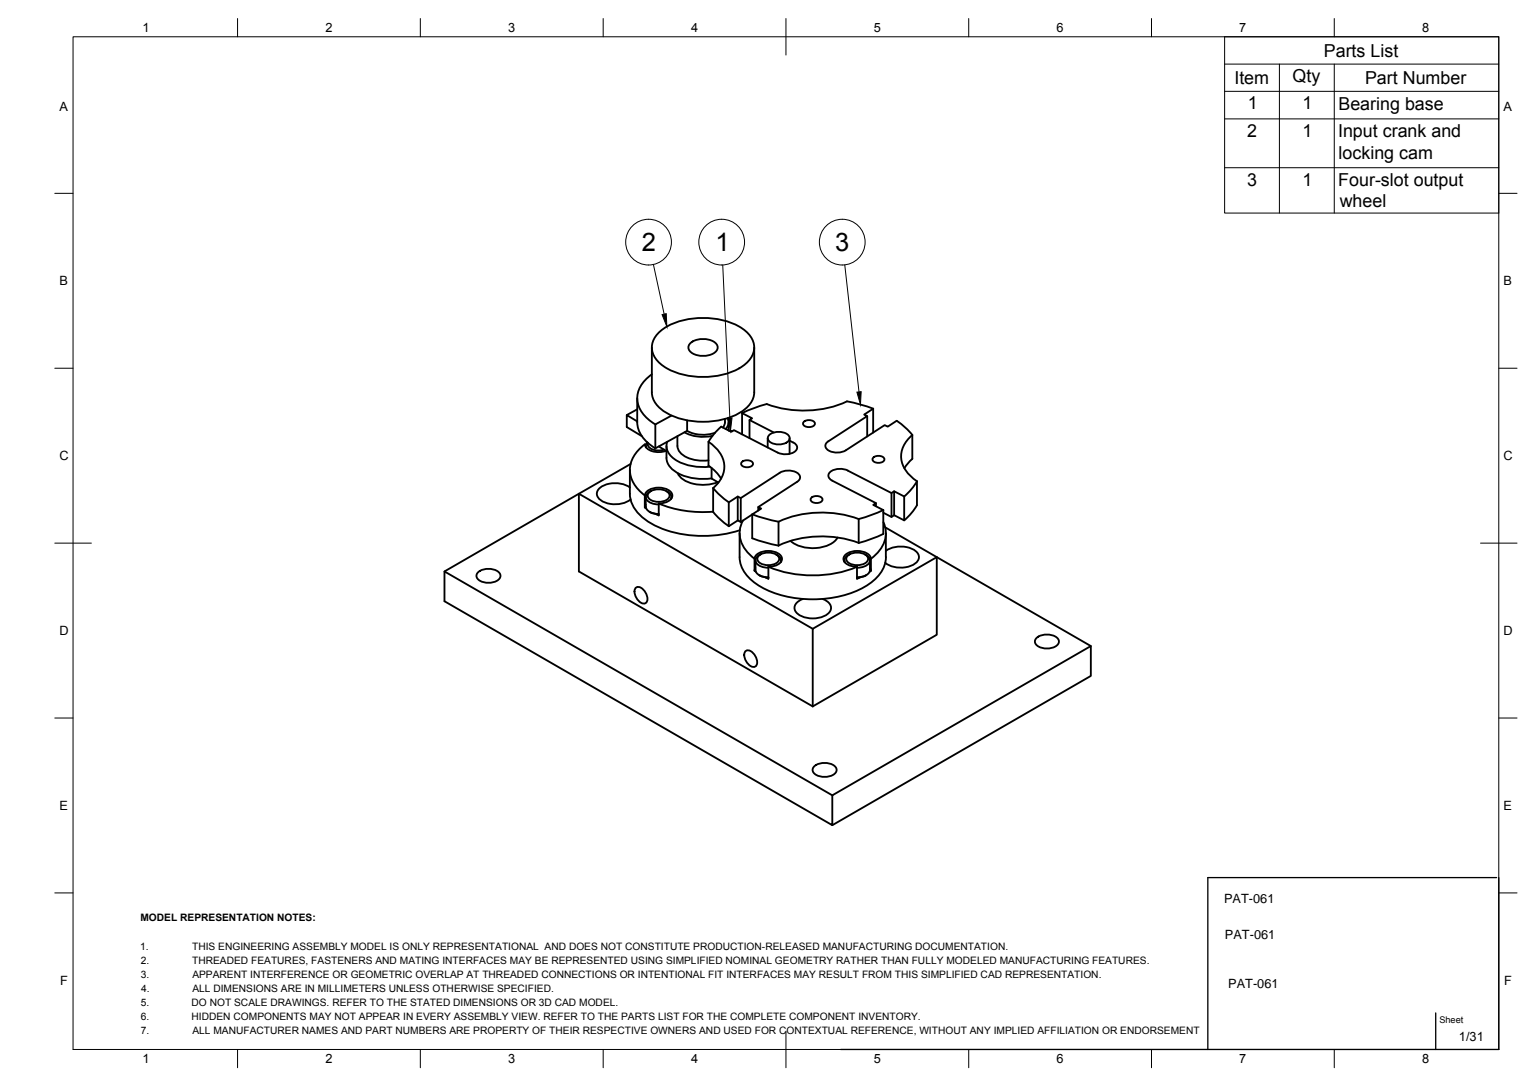
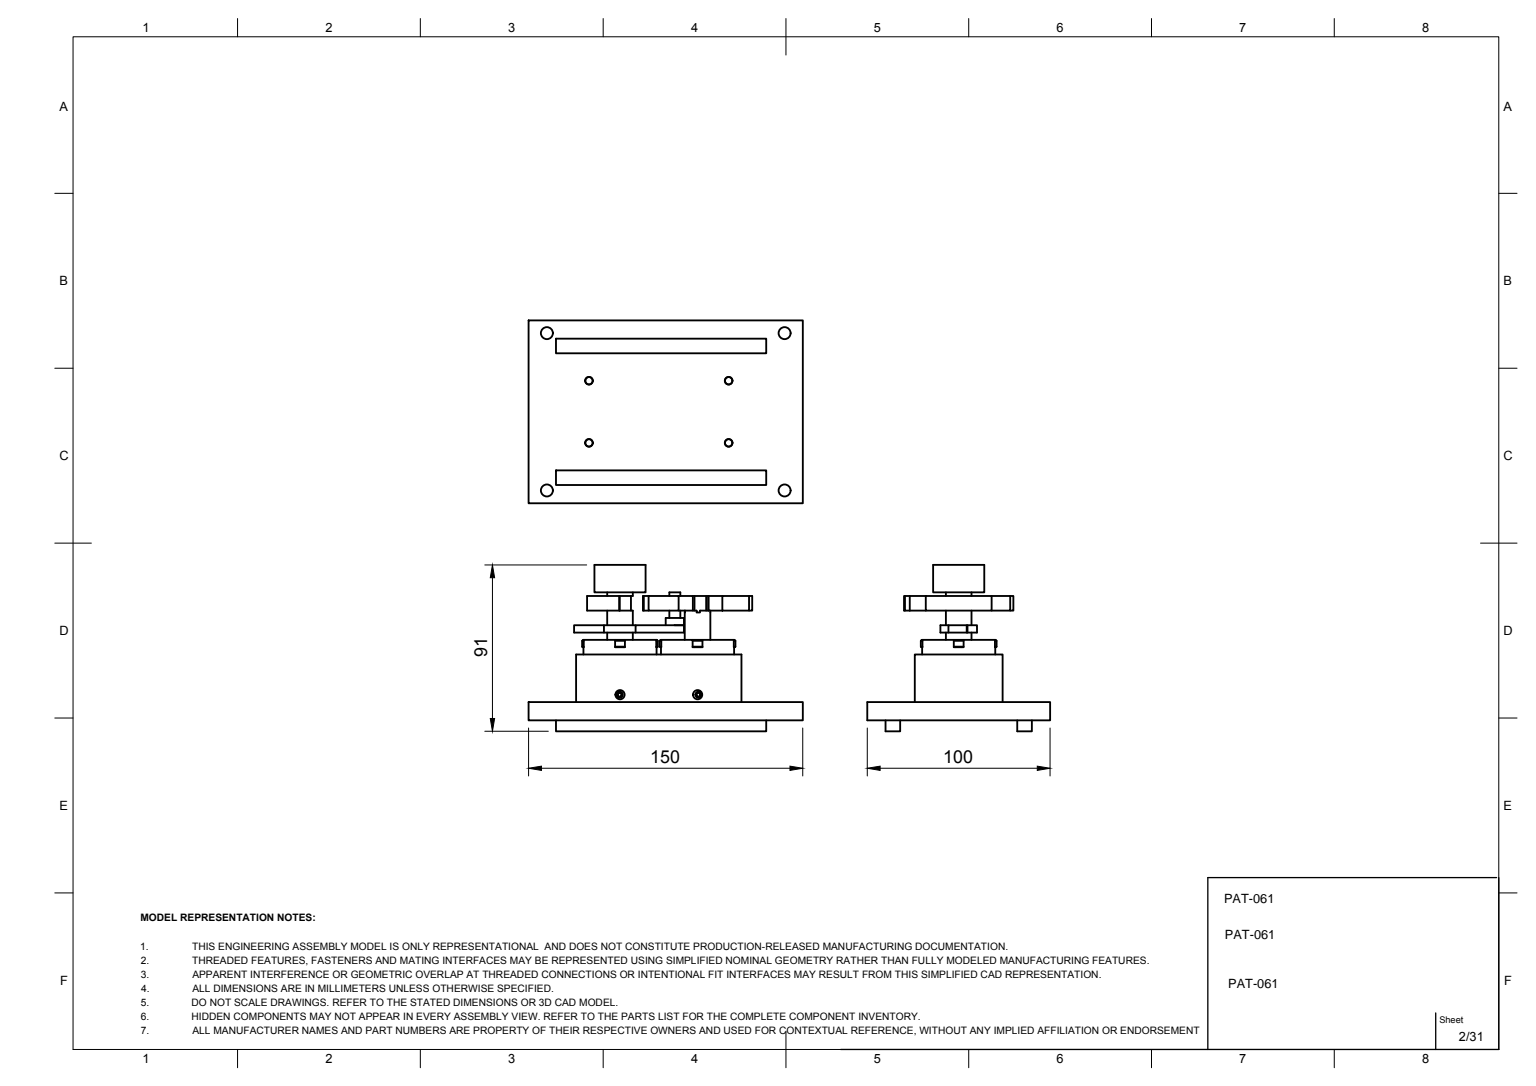
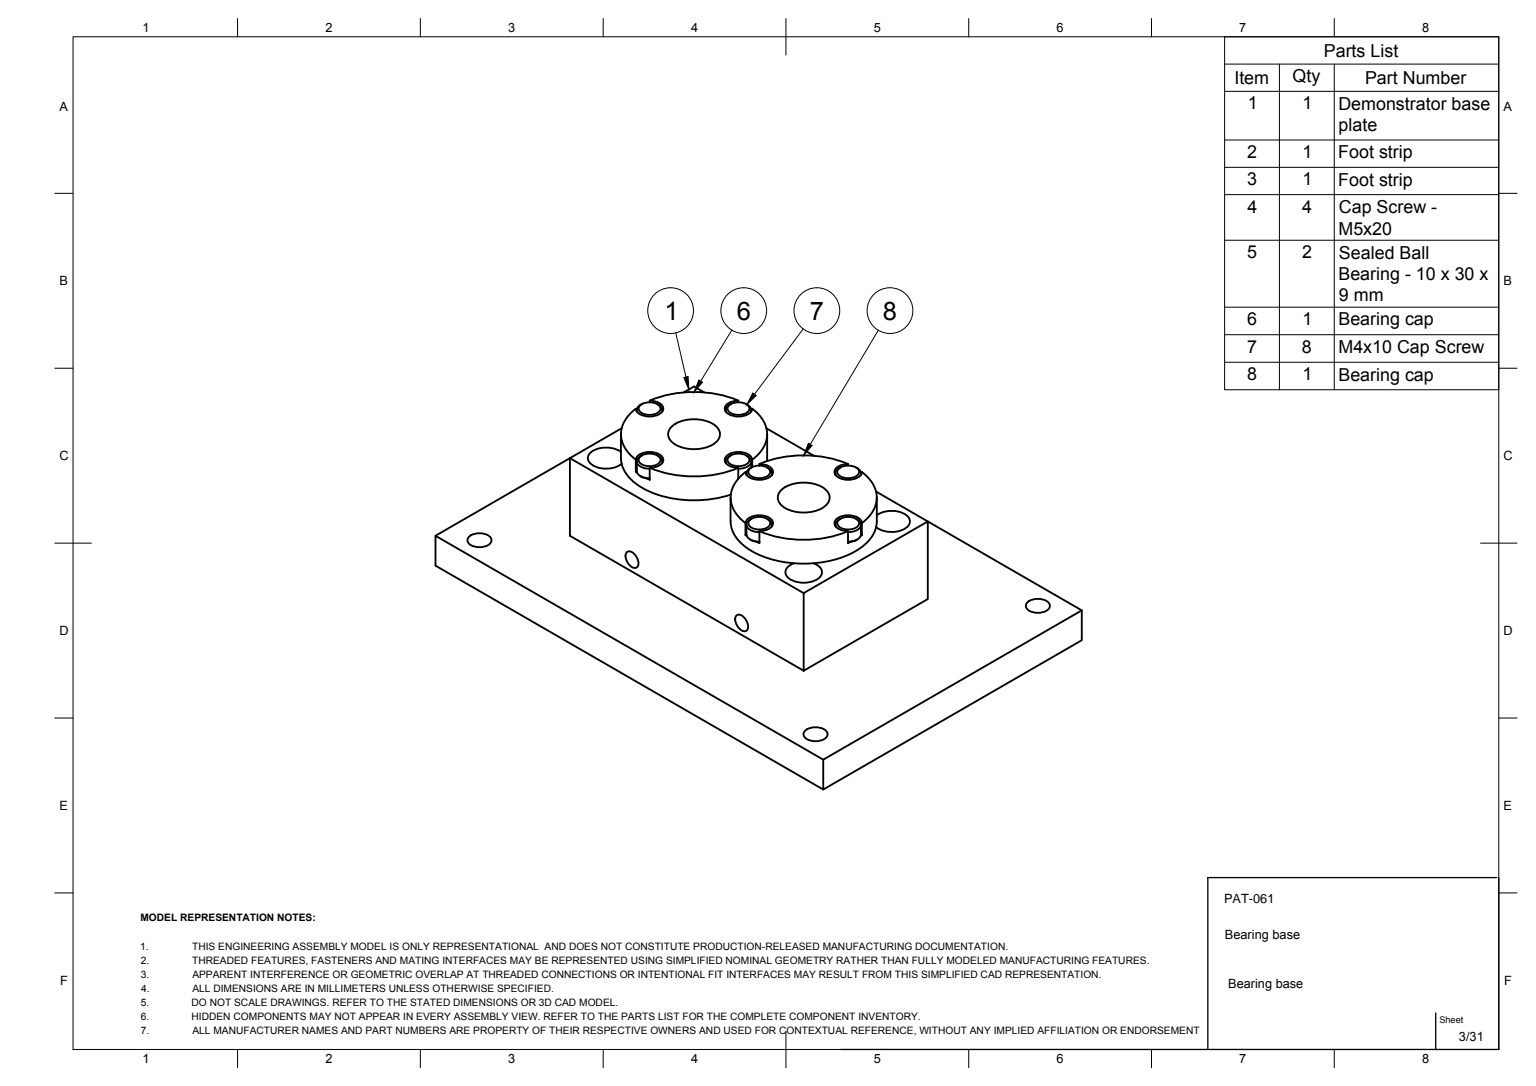
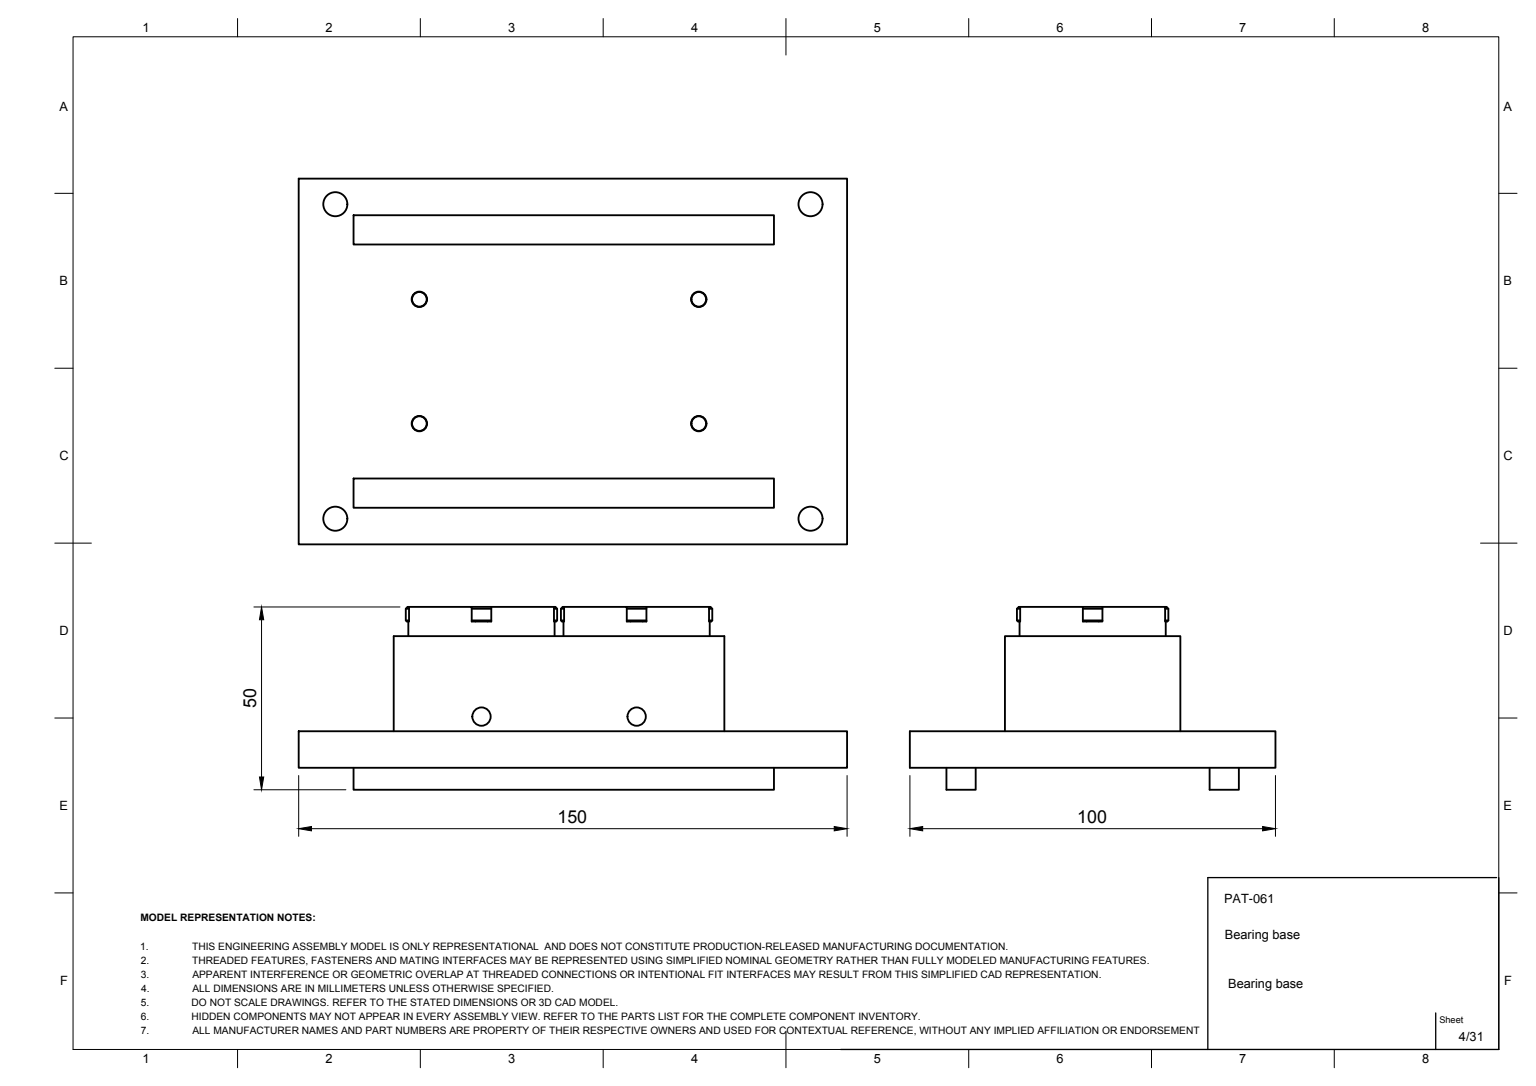
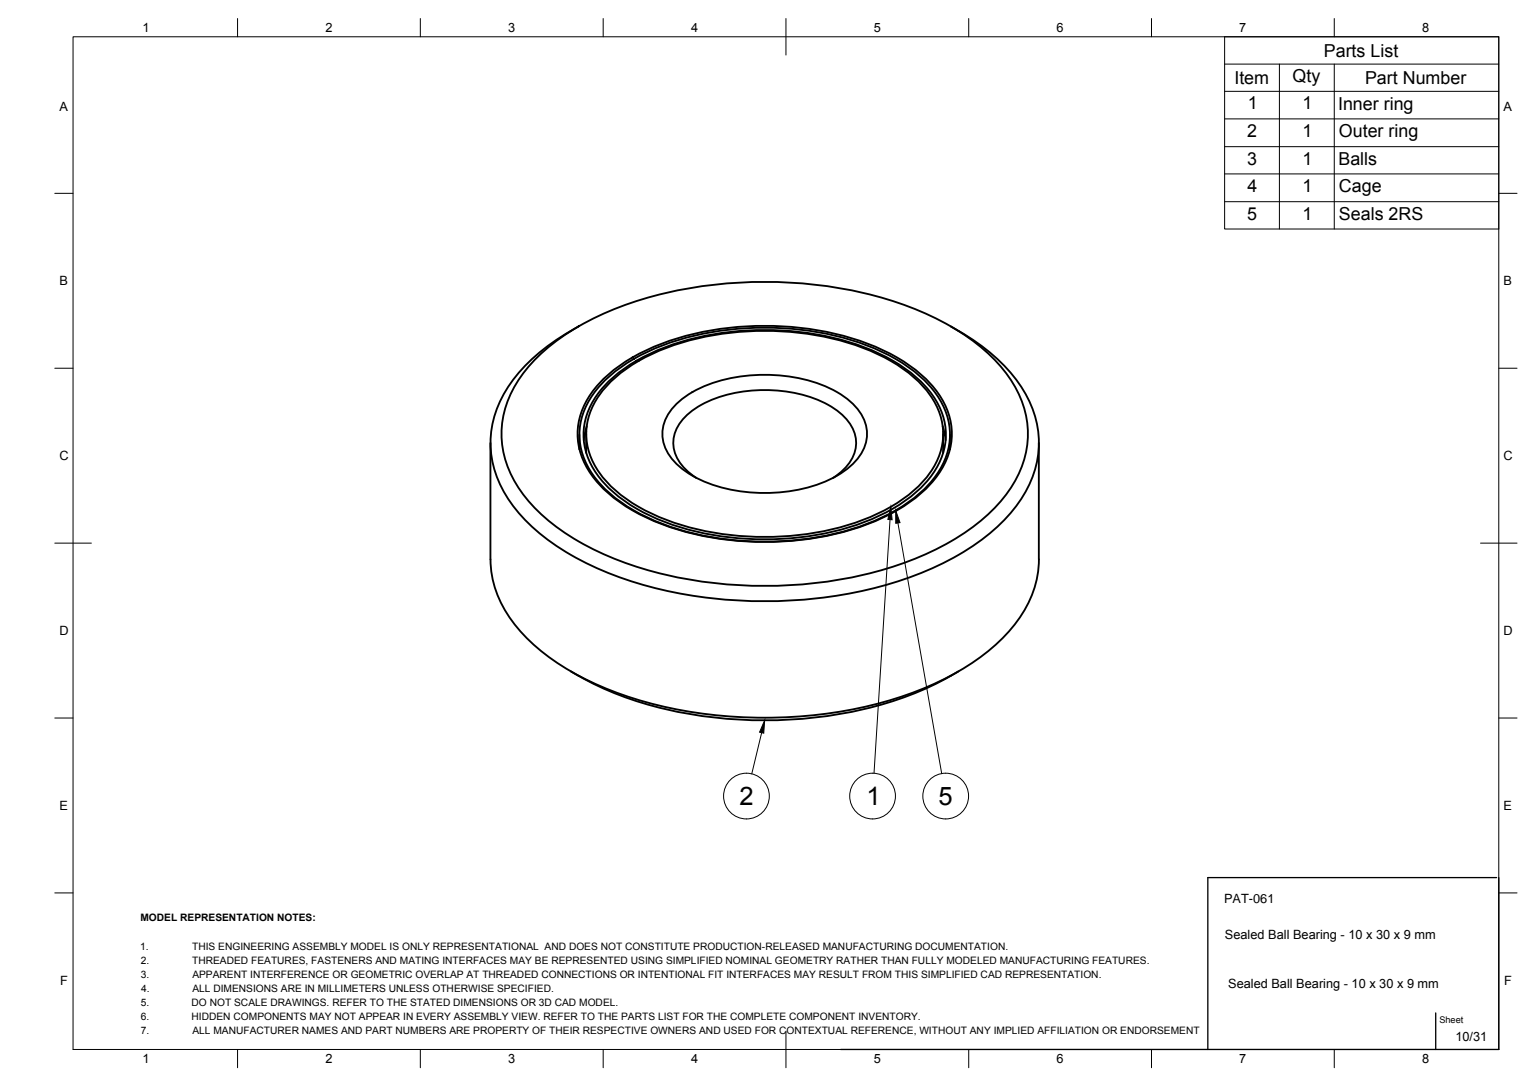
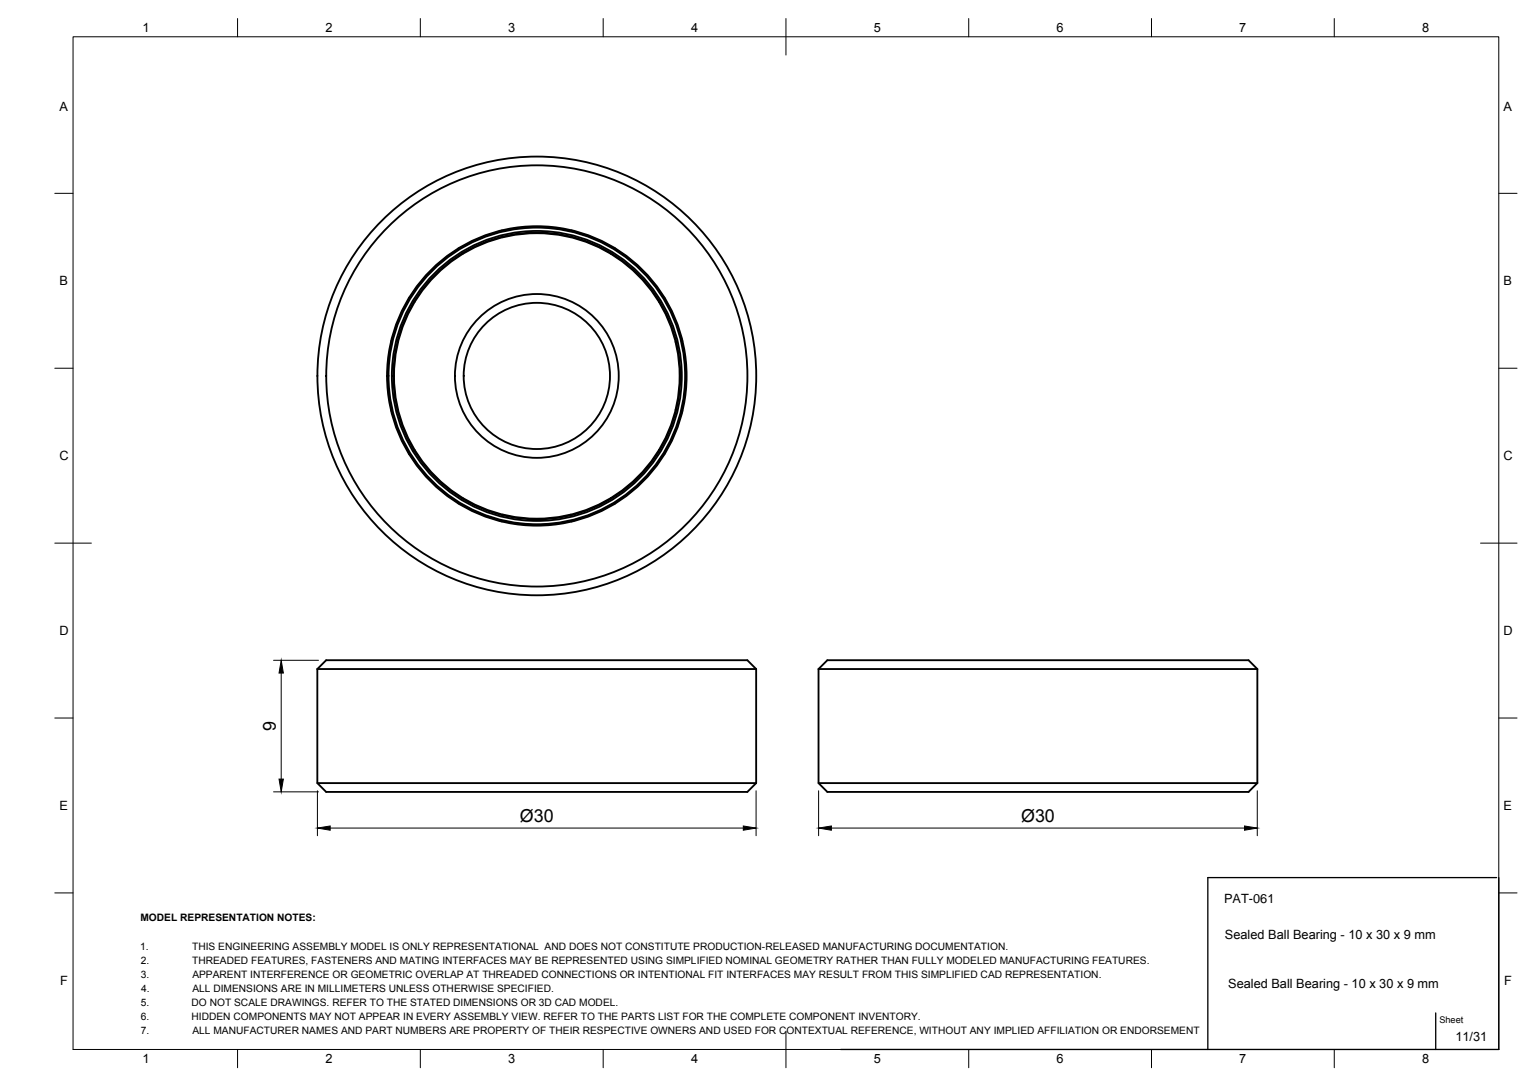
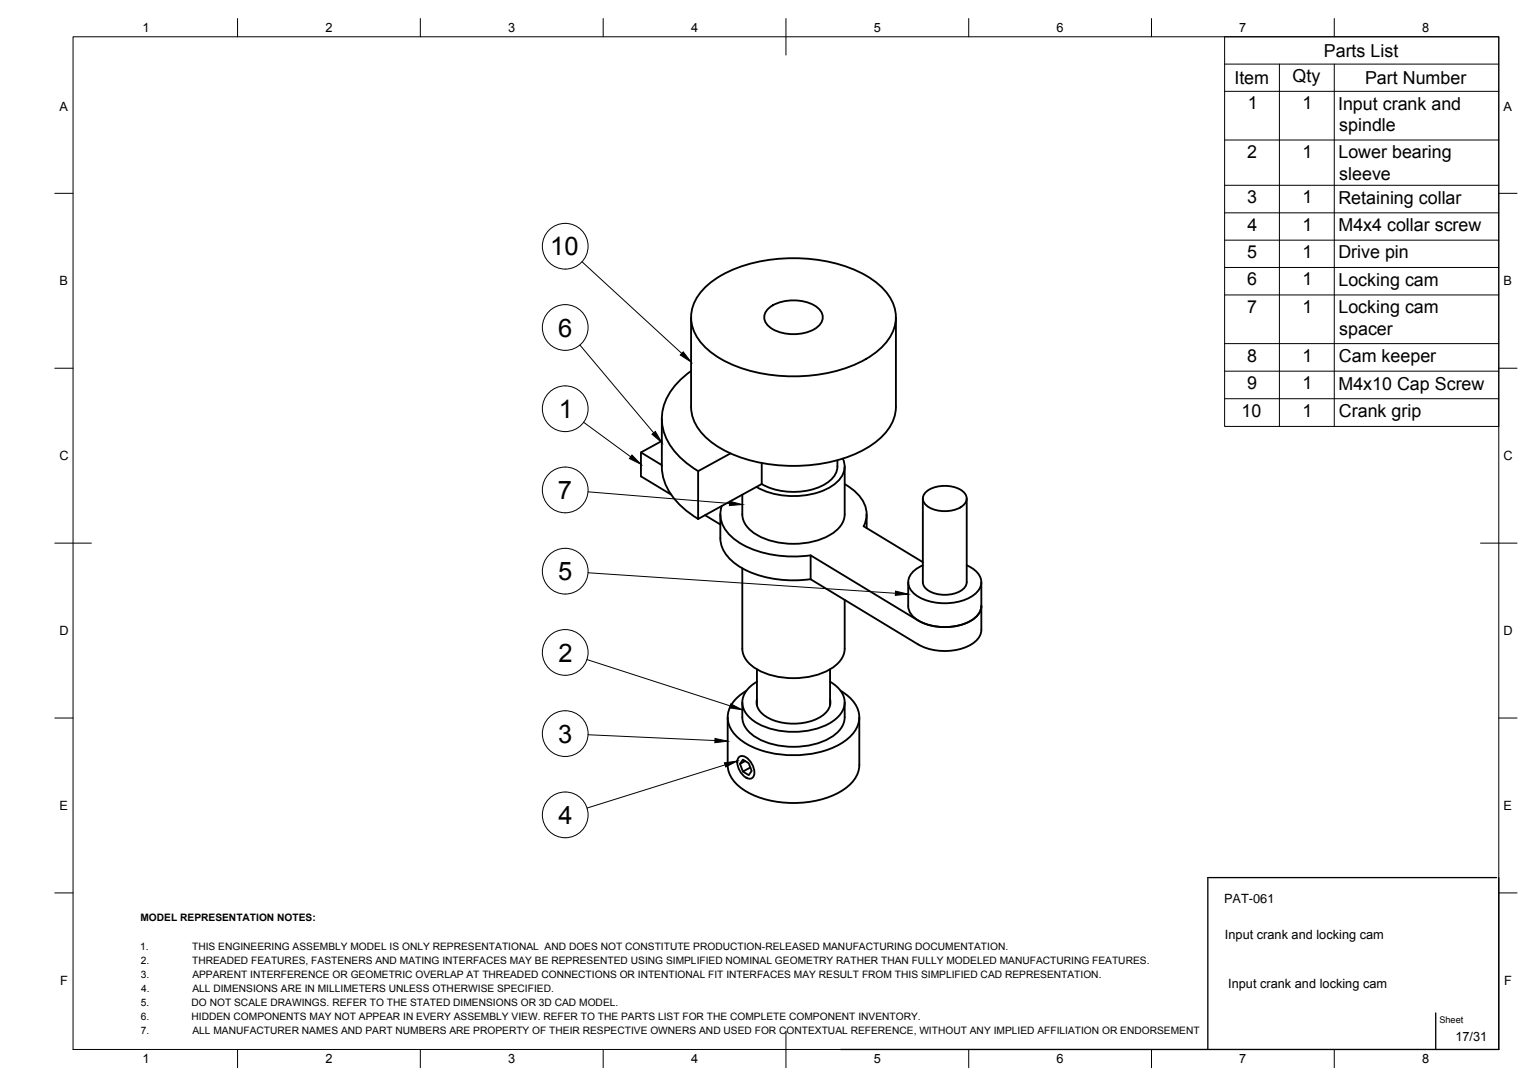
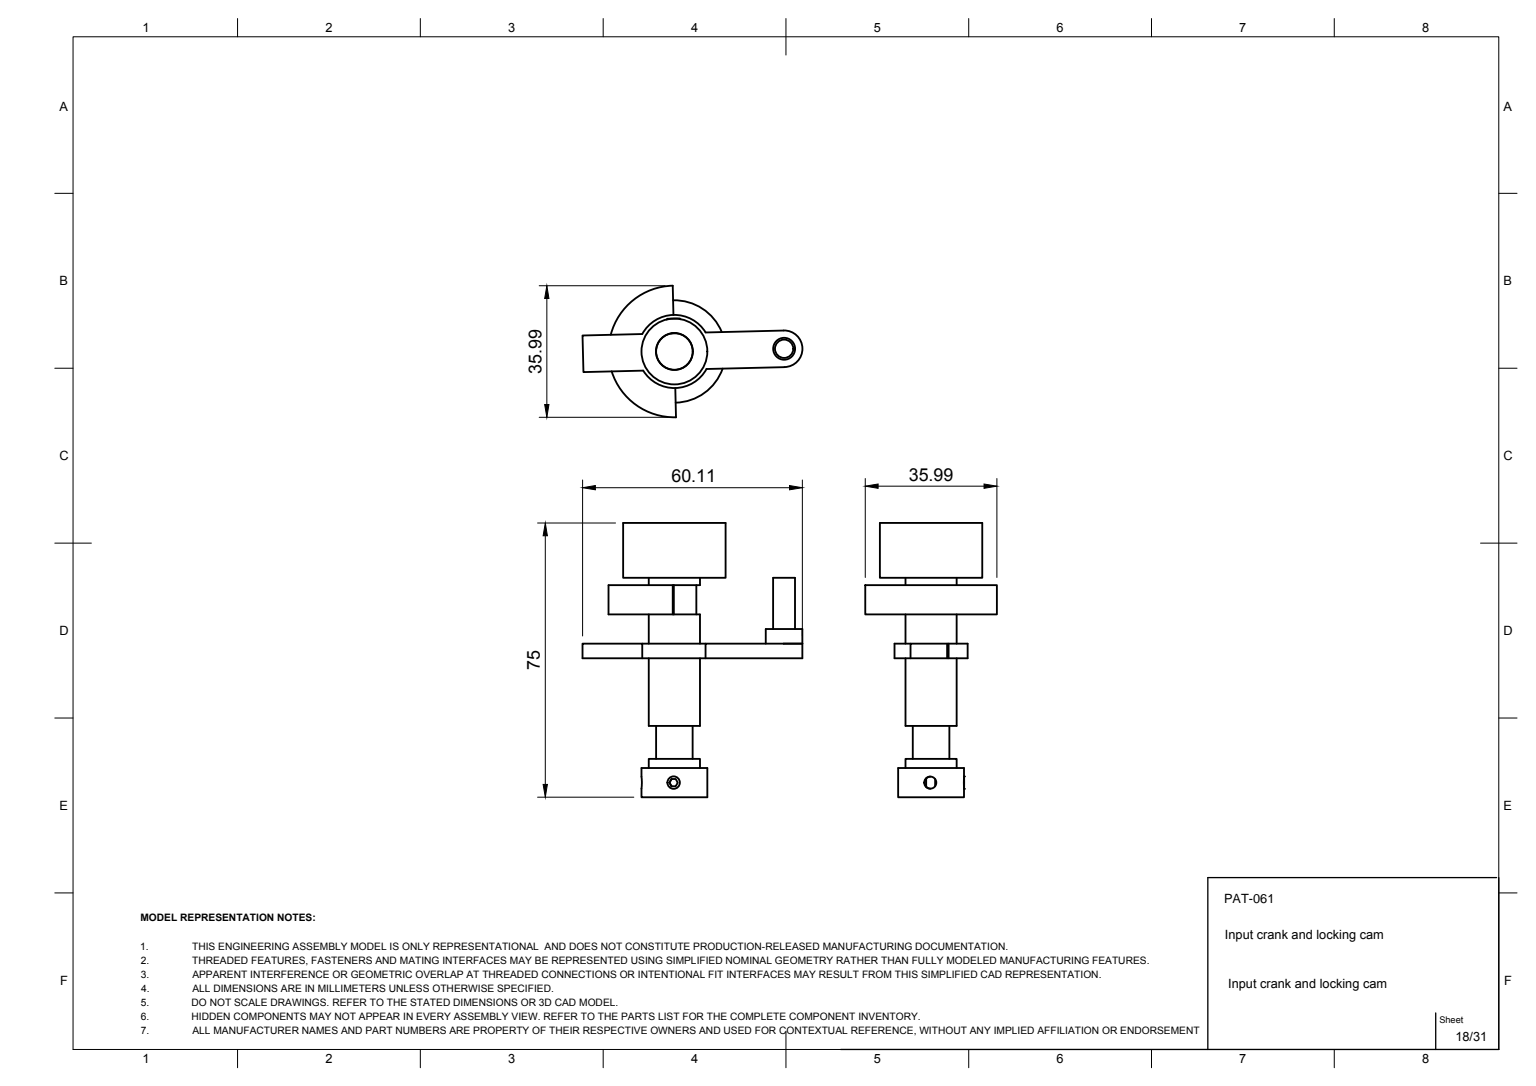
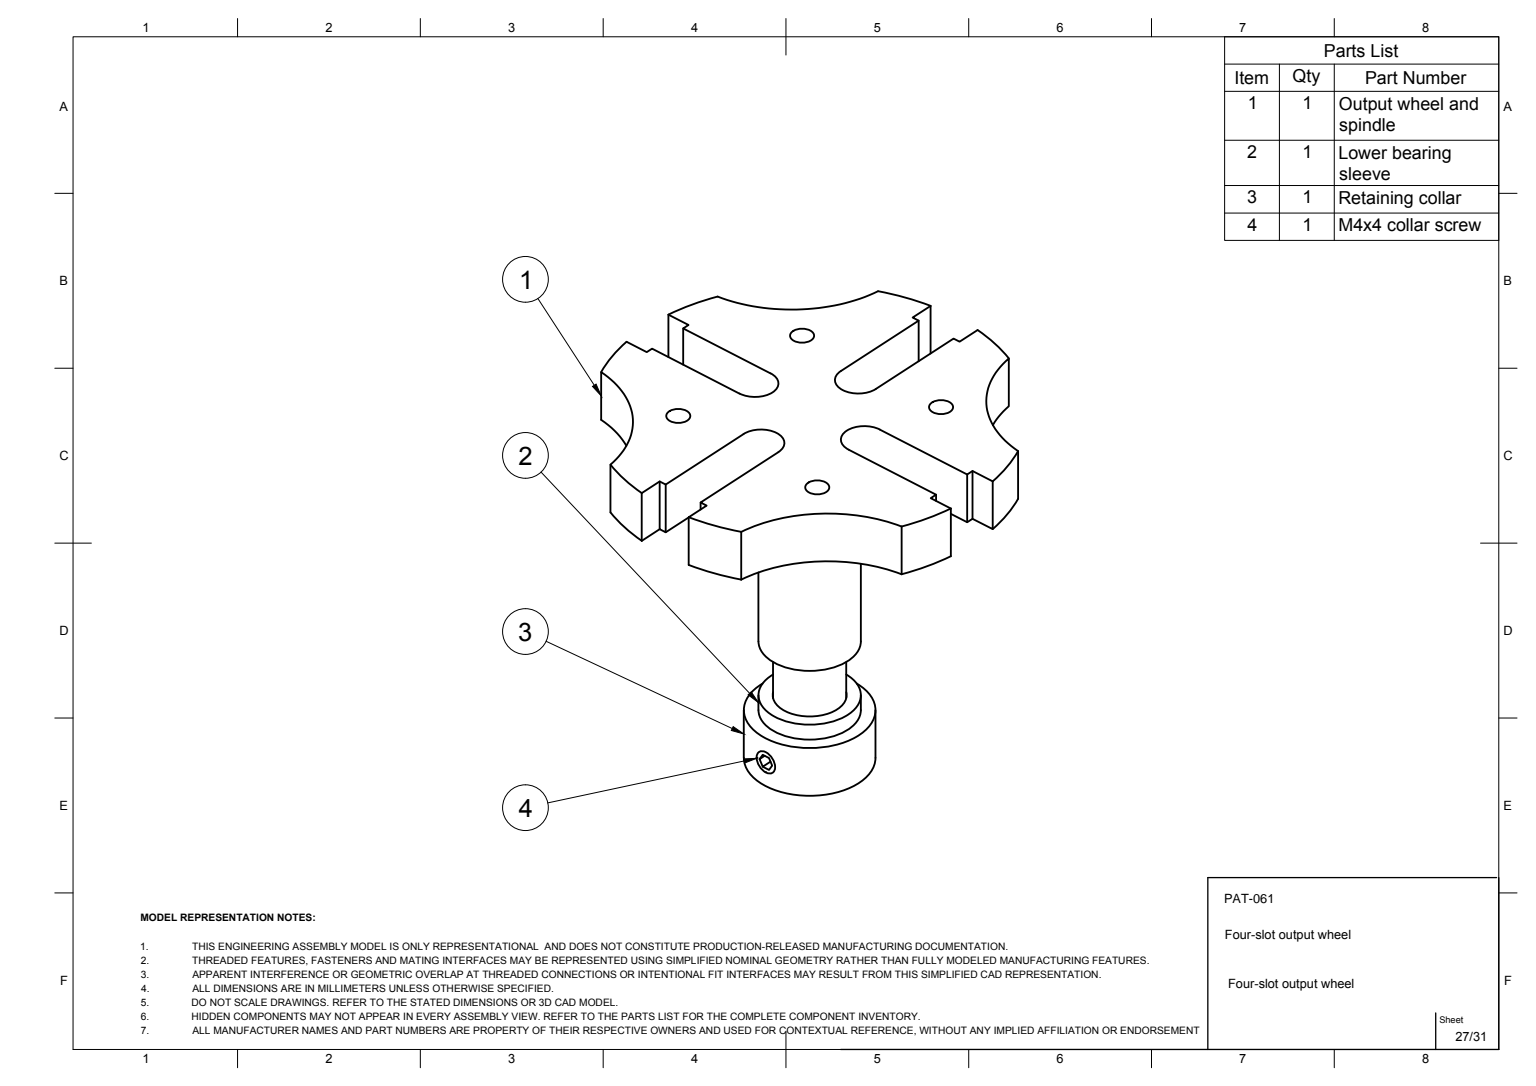
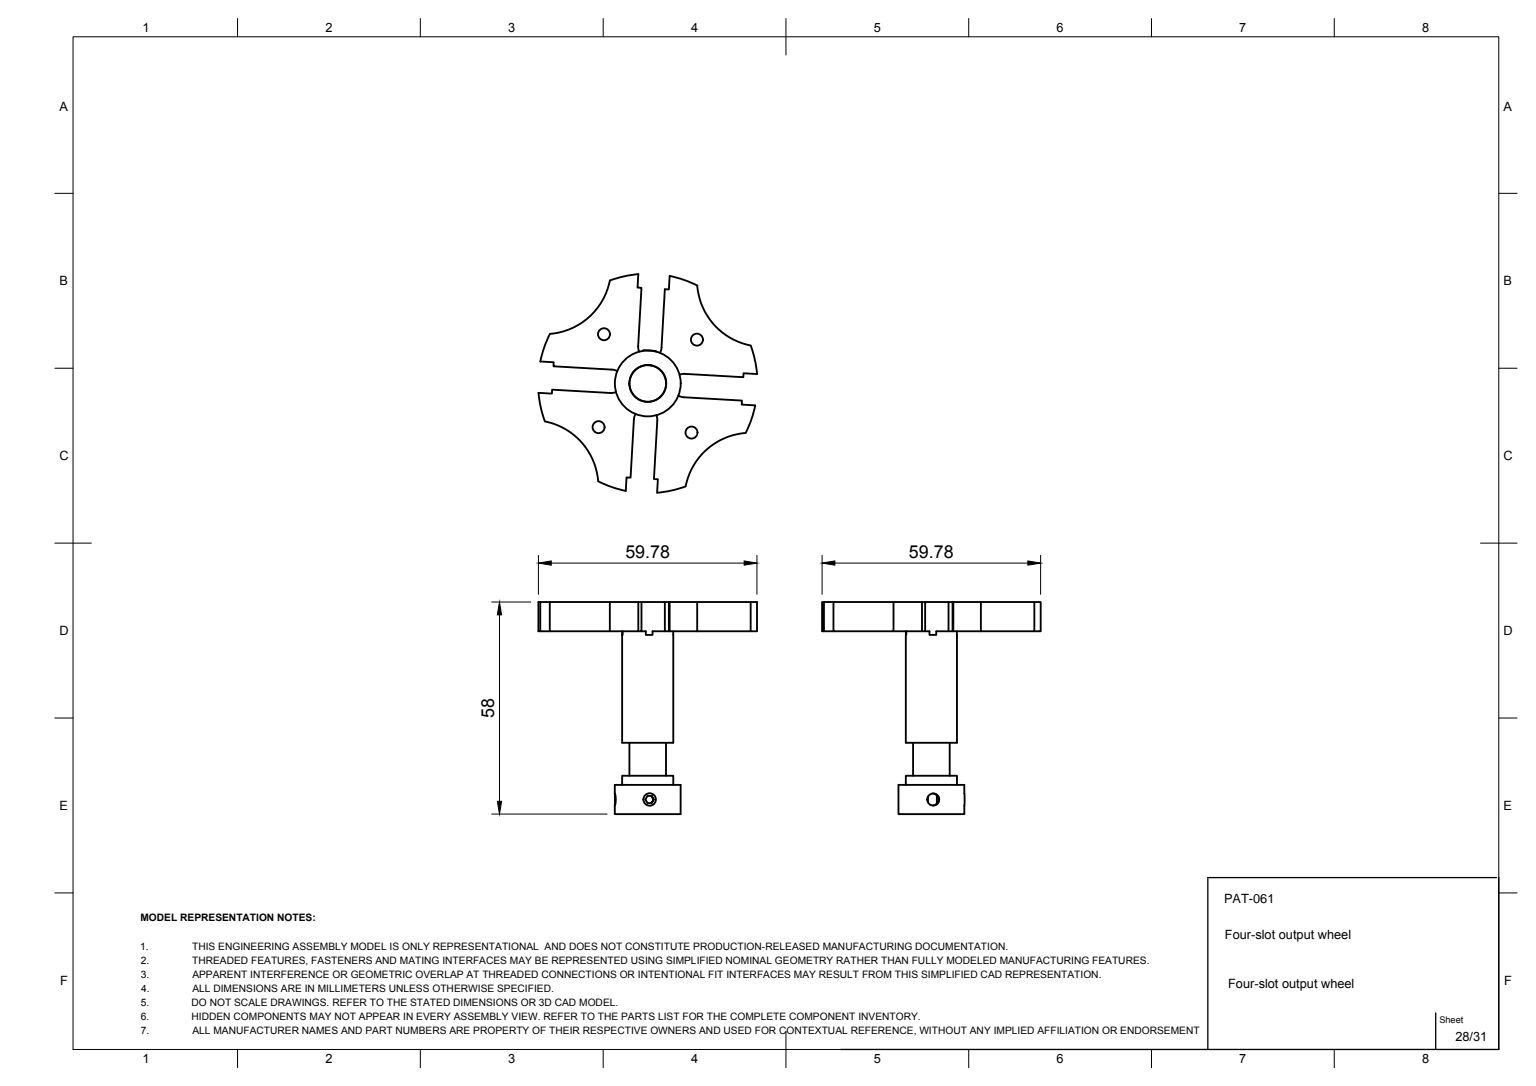
ISO-10303-21;
HEADER;
/* Generated by software containing ST-Developer
 * from STEP Tools, Inc. (www.steptools.com) 
 */

FILE_DESCRIPTION(
/* description */ ('Compact intermittent indexer'),
/* implementation_level */ '2;1');

FILE_NAME(
/* name */ 'PAT-061',
/* time_stamp */ '2026-10-29T16:32:17-07:00',
/* author */ (''),
/* organization */ (''),
/* preprocessor_version */ 'ST-DEVELOPER v20.2',
/* originating_system */ 'Autodesk Translation Framework v15.17.0.0',
/* authorisation */ '');

FILE_SCHEMA (('AUTOMOTIVE_DESIGN { 1 0 10303 214 3 1 1 }'));
ENDSEC;

DATA;
#10=MECHANICAL_DESIGN_GEOMETRIC_PRESENTATION_REPRESENTATION('',(#257,#258,
#259,#260,#261,#262,#263,#264,#265,#266,#267,#268,#269,#270,#271,#272,#273,
#274,#275,#276,#277,#278,#279,#280,#281,#282,#283,#284,#285,#286,#287,#288),
#10837);
#11=ITEM_DEFINED_TRANSFORMATION($,$,#6189,#6317);
#12=ITEM_DEFINED_TRANSFORMATION($,$,#6209,#6318);
#13=ITEM_DEFINED_TRANSFORMATION($,$,#6229,#6319);
#14=ITEM_DEFINED_TRANSFORMATION($,$,#6246,#6320);
#15=ITEM_DEFINED_TRANSFORMATION($,$,#6300,#6321);
#16=ITEM_DEFINED_TRANSFORMATION($,$,#5930,#6467);
#17=ITEM_DEFINED_TRANSFORMATION($,$,#6050,#6468);
#18=ITEM_DEFINED_TRANSFORMATION($,$,#6057,#6469);
#19=ITEM_DEFINED_TRANSFORMATION($,$,#6064,#6470);
#20=ITEM_DEFINED_TRANSFORMATION($,$,#6113,#6471);
#21=ITEM_DEFINED_TRANSFORMATION($,$,#6162,#6472);
#22=ITEM_DEFINED_TRANSFORMATION($,$,#6162,#6473);
#23=ITEM_DEFINED_TRANSFORMATION($,$,#6162,#6474);
#24=ITEM_DEFINED_TRANSFORMATION($,$,#6162,#6475);
#25=ITEM_DEFINED_TRANSFORMATION($,$,#6188,#6476);
#26=ITEM_DEFINED_TRANSFORMATION($,$,#6443,#6477);
#27=ITEM_DEFINED_TRANSFORMATION($,$,#6443,#6478);
#28=ITEM_DEFINED_TRANSFORMATION($,$,#6443,#6479);
#29=ITEM_DEFINED_TRANSFORMATION($,$,#6443,#6480);
#30=ITEM_DEFINED_TRANSFORMATION($,$,#6188,#6481);
#31=ITEM_DEFINED_TRANSFORMATION($,$,#6443,#6482);
#32=ITEM_DEFINED_TRANSFORMATION($,$,#6443,#6483);
#33=ITEM_DEFINED_TRANSFORMATION($,$,#6443,#6484);
#34=ITEM_DEFINED_TRANSFORMATION($,$,#6443,#6485);
#35=ITEM_DEFINED_TRANSFORMATION($,$,#6323,#6649);
#36=ITEM_DEFINED_TRANSFORMATION($,$,#6359,#6650);
#37=ITEM_DEFINED_TRANSFORMATION($,$,#6368,#6651);
#38=ITEM_DEFINED_TRANSFORMATION($,$,#6388,#6652);
#39=ITEM_DEFINED_TRANSFORMATION($,$,#6402,#6653);
#40=ITEM_DEFINED_TRANSFORMATION($,$,#6416,#6654);
#41=ITEM_DEFINED_TRANSFORMATION($,$,#6425,#6655);
#42=ITEM_DEFINED_TRANSFORMATION($,$,#6434,#6656);
#43=ITEM_DEFINED_TRANSFORMATION($,$,#6634,#6657);
#44=ITEM_DEFINED_TRANSFORMATION($,$,#6443,#6658);
#45=ITEM_DEFINED_TRANSFORMATION($,$,#6487,#6659);
#46=ITEM_DEFINED_TRANSFORMATION($,$,#6605,#6660);
#47=ITEM_DEFINED_TRANSFORMATION($,$,#6614,#6661);
#48=ITEM_DEFINED_TRANSFORMATION($,$,#6634,#6662);
#49=ITEM_DEFINED_TRANSFORMATION($,$,#5929,#6663);
#50=ITEM_DEFINED_TRANSFORMATION($,$,#6322,#6664);
#51=ITEM_DEFINED_TRANSFORMATION($,$,#6486,#6665);
#52=(
REPRESENTATION_RELATIONSHIP($,$,#10950,#10949)
REPRESENTATION_RELATIONSHIP_WITH_TRANSFORMATION(#11)
SHAPE_REPRESENTATION_RELATIONSHIP()
);
#53=(
REPRESENTATION_RELATIONSHIP($,$,#10951,#10949)
REPRESENTATION_RELATIONSHIP_WITH_TRANSFORMATION(#12)
SHAPE_REPRESENTATION_RELATIONSHIP()
);
#54=(
REPRESENTATION_RELATIONSHIP($,$,#10952,#10949)
REPRESENTATION_RELATIONSHIP_WITH_TRANSFORMATION(#13)
SHAPE_REPRESENTATION_RELATIONSHIP()
);
#55=(
REPRESENTATION_RELATIONSHIP($,$,#10953,#10949)
REPRESENTATION_RELATIONSHIP_WITH_TRANSFORMATION(#14)
SHAPE_REPRESENTATION_RELATIONSHIP()
);
#56=(
REPRESENTATION_RELATIONSHIP($,$,#10954,#10949)
REPRESENTATION_RELATIONSHIP_WITH_TRANSFORMATION(#15)
SHAPE_REPRESENTATION_RELATIONSHIP()
);
#57=(
REPRESENTATION_RELATIONSHIP($,$,#10943,#10942)
REPRESENTATION_RELATIONSHIP_WITH_TRANSFORMATION(#16)
SHAPE_REPRESENTATION_RELATIONSHIP()
);
#58=(
REPRESENTATION_RELATIONSHIP($,$,#10944,#10942)
REPRESENTATION_RELATIONSHIP_WITH_TRANSFORMATION(#17)
SHAPE_REPRESENTATION_RELATIONSHIP()
);
#59=(
REPRESENTATION_RELATIONSHIP($,$,#10945,#10942)
REPRESENTATION_RELATIONSHIP_WITH_TRANSFORMATION(#18)
SHAPE_REPRESENTATION_RELATIONSHIP()
);
#60=(
REPRESENTATION_RELATIONSHIP($,$,#10946,#10942)
REPRESENTATION_RELATIONSHIP_WITH_TRANSFORMATION(#19)
SHAPE_REPRESENTATION_RELATIONSHIP()
);
#61=(
REPRESENTATION_RELATIONSHIP($,$,#10947,#10942)
REPRESENTATION_RELATIONSHIP_WITH_TRANSFORMATION(#20)
SHAPE_REPRESENTATION_RELATIONSHIP()
);
#62=(
REPRESENTATION_RELATIONSHIP($,$,#10948,#10942)
REPRESENTATION_RELATIONSHIP_WITH_TRANSFORMATION(#21)
SHAPE_REPRESENTATION_RELATIONSHIP()
);
#63=(
REPRESENTATION_RELATIONSHIP($,$,#10948,#10942)
REPRESENTATION_RELATIONSHIP_WITH_TRANSFORMATION(#22)
SHAPE_REPRESENTATION_RELATIONSHIP()
);
#64=(
REPRESENTATION_RELATIONSHIP($,$,#10948,#10942)
REPRESENTATION_RELATIONSHIP_WITH_TRANSFORMATION(#23)
SHAPE_REPRESENTATION_RELATIONSHIP()
);
#65=(
REPRESENTATION_RELATIONSHIP($,$,#10948,#10942)
REPRESENTATION_RELATIONSHIP_WITH_TRANSFORMATION(#24)
SHAPE_REPRESENTATION_RELATIONSHIP()
);
#66=(
REPRESENTATION_RELATIONSHIP($,$,#10949,#10942)
REPRESENTATION_RELATIONSHIP_WITH_TRANSFORMATION(#25)
SHAPE_REPRESENTATION_RELATIONSHIP()
);
#67=(
REPRESENTATION_RELATIONSHIP($,$,#10964,#10942)
REPRESENTATION_RELATIONSHIP_WITH_TRANSFORMATION(#26)
SHAPE_REPRESENTATION_RELATIONSHIP()
);
#68=(
REPRESENTATION_RELATIONSHIP($,$,#10964,#10942)
REPRESENTATION_RELATIONSHIP_WITH_TRANSFORMATION(#27)
SHAPE_REPRESENTATION_RELATIONSHIP()
);
#69=(
REPRESENTATION_RELATIONSHIP($,$,#10964,#10942)
REPRESENTATION_RELATIONSHIP_WITH_TRANSFORMATION(#28)
SHAPE_REPRESENTATION_RELATIONSHIP()
);
#70=(
REPRESENTATION_RELATIONSHIP($,$,#10964,#10942)
REPRESENTATION_RELATIONSHIP_WITH_TRANSFORMATION(#29)
SHAPE_REPRESENTATION_RELATIONSHIP()
);
#71=(
REPRESENTATION_RELATIONSHIP($,$,#10949,#10942)
REPRESENTATION_RELATIONSHIP_WITH_TRANSFORMATION(#30)
SHAPE_REPRESENTATION_RELATIONSHIP()
);
#72=(
REPRESENTATION_RELATIONSHIP($,$,#10964,#10942)
REPRESENTATION_RELATIONSHIP_WITH_TRANSFORMATION(#31)
SHAPE_REPRESENTATION_RELATIONSHIP()
);
#73=(
REPRESENTATION_RELATIONSHIP($,$,#10964,#10942)
REPRESENTATION_RELATIONSHIP_WITH_TRANSFORMATION(#32)
SHAPE_REPRESENTATION_RELATIONSHIP()
);
#74=(
REPRESENTATION_RELATIONSHIP($,$,#10964,#10942)
REPRESENTATION_RELATIONSHIP_WITH_TRANSFORMATION(#33)
SHAPE_REPRESENTATION_RELATIONSHIP()
);
#75=(
REPRESENTATION_RELATIONSHIP($,$,#10964,#10942)
REPRESENTATION_RELATIONSHIP_WITH_TRANSFORMATION(#34)
SHAPE_REPRESENTATION_RELATIONSHIP()
);
#76=(
REPRESENTATION_RELATIONSHIP($,$,#10956,#10955)
REPRESENTATION_RELATIONSHIP_WITH_TRANSFORMATION(#35)
SHAPE_REPRESENTATION_RELATIONSHIP()
);
#77=(
REPRESENTATION_RELATIONSHIP($,$,#10957,#10955)
REPRESENTATION_RELATIONSHIP_WITH_TRANSFORMATION(#36)
SHAPE_REPRESENTATION_RELATIONSHIP()
);
#78=(
REPRESENTATION_RELATIONSHIP($,$,#10958,#10955)
REPRESENTATION_RELATIONSHIP_WITH_TRANSFORMATION(#37)
SHAPE_REPRESENTATION_RELATIONSHIP()
);
#79=(
REPRESENTATION_RELATIONSHIP($,$,#10959,#10955)
REPRESENTATION_RELATIONSHIP_WITH_TRANSFORMATION(#38)
SHAPE_REPRESENTATION_RELATIONSHIP()
);
#80=(
REPRESENTATION_RELATIONSHIP($,$,#10960,#10955)
REPRESENTATION_RELATIONSHIP_WITH_TRANSFORMATION(#39)
SHAPE_REPRESENTATION_RELATIONSHIP()
);
#81=(
REPRESENTATION_RELATIONSHIP($,$,#10961,#10955)
REPRESENTATION_RELATIONSHIP_WITH_TRANSFORMATION(#40)
SHAPE_REPRESENTATION_RELATIONSHIP()
);
#82=(
REPRESENTATION_RELATIONSHIP($,$,#10962,#10955)
REPRESENTATION_RELATIONSHIP_WITH_TRANSFORMATION(#41)
SHAPE_REPRESENTATION_RELATIONSHIP()
);
#83=(
REPRESENTATION_RELATIONSHIP($,$,#10963,#10955)
REPRESENTATION_RELATIONSHIP_WITH_TRANSFORMATION(#42)
SHAPE_REPRESENTATION_RELATIONSHIP()
);
#84=(
REPRESENTATION_RELATIONSHIP($,$,#10969,#10955)
REPRESENTATION_RELATIONSHIP_WITH_TRANSFORMATION(#43)
SHAPE_REPRESENTATION_RELATIONSHIP()
);
#85=(
REPRESENTATION_RELATIONSHIP($,$,#10964,#10955)
REPRESENTATION_RELATIONSHIP_WITH_TRANSFORMATION(#44)
SHAPE_REPRESENTATION_RELATIONSHIP()
);
#86=(
REPRESENTATION_RELATIONSHIP($,$,#10966,#10965)
REPRESENTATION_RELATIONSHIP_WITH_TRANSFORMATION(#45)
SHAPE_REPRESENTATION_RELATIONSHIP()
);
#87=(
REPRESENTATION_RELATIONSHIP($,$,#10967,#10965)
REPRESENTATION_RELATIONSHIP_WITH_TRANSFORMATION(#46)
SHAPE_REPRESENTATION_RELATIONSHIP()
);
#88=(
REPRESENTATION_RELATIONSHIP($,$,#10968,#10965)
REPRESENTATION_RELATIONSHIP_WITH_TRANSFORMATION(#47)
SHAPE_REPRESENTATION_RELATIONSHIP()
);
#89=(
REPRESENTATION_RELATIONSHIP($,$,#10969,#10965)
REPRESENTATION_RELATIONSHIP_WITH_TRANSFORMATION(#48)
SHAPE_REPRESENTATION_RELATIONSHIP()
);
#90=(
REPRESENTATION_RELATIONSHIP($,$,#10942,#10941)
REPRESENTATION_RELATIONSHIP_WITH_TRANSFORMATION(#49)
SHAPE_REPRESENTATION_RELATIONSHIP()
);
#91=(
REPRESENTATION_RELATIONSHIP($,$,#10955,#10941)
REPRESENTATION_RELATIONSHIP_WITH_TRANSFORMATION(#50)
SHAPE_REPRESENTATION_RELATIONSHIP()
);
#92=(
REPRESENTATION_RELATIONSHIP($,$,#10965,#10941)
REPRESENTATION_RELATIONSHIP_WITH_TRANSFORMATION(#51)
SHAPE_REPRESENTATION_RELATIONSHIP()
);
#93=CONTEXT_DEPENDENT_SHAPE_REPRESENTATION(#52,#10885);
#94=CONTEXT_DEPENDENT_SHAPE_REPRESENTATION(#53,#10886);
#95=CONTEXT_DEPENDENT_SHAPE_REPRESENTATION(#54,#10887);
#96=CONTEXT_DEPENDENT_SHAPE_REPRESENTATION(#55,#10888);
#97=CONTEXT_DEPENDENT_SHAPE_REPRESENTATION(#56,#10889);
#98=CONTEXT_DEPENDENT_SHAPE_REPRESENTATION(#57,#10900);
#99=CONTEXT_DEPENDENT_SHAPE_REPRESENTATION(#58,#10901);
#100=CONTEXT_DEPENDENT_SHAPE_REPRESENTATION(#59,#10902);
#101=CONTEXT_DEPENDENT_SHAPE_REPRESENTATION(#60,#10903);
#102=CONTEXT_DEPENDENT_SHAPE_REPRESENTATION(#61,#10904);
#103=CONTEXT_DEPENDENT_SHAPE_REPRESENTATION(#62,#10905);
#104=CONTEXT_DEPENDENT_SHAPE_REPRESENTATION(#63,#10906);
#105=CONTEXT_DEPENDENT_SHAPE_REPRESENTATION(#64,#10907);
#106=CONTEXT_DEPENDENT_SHAPE_REPRESENTATION(#65,#10908);
#107=CONTEXT_DEPENDENT_SHAPE_REPRESENTATION(#66,#10909);
#108=CONTEXT_DEPENDENT_SHAPE_REPRESENTATION(#67,#10910);
#109=CONTEXT_DEPENDENT_SHAPE_REPRESENTATION(#68,#10911);
#110=CONTEXT_DEPENDENT_SHAPE_REPRESENTATION(#69,#10912);
#111=CONTEXT_DEPENDENT_SHAPE_REPRESENTATION(#70,#10913);
#112=CONTEXT_DEPENDENT_SHAPE_REPRESENTATION(#71,#10914);
#113=CONTEXT_DEPENDENT_SHAPE_REPRESENTATION(#72,#10915);
#114=CONTEXT_DEPENDENT_SHAPE_REPRESENTATION(#73,#10916);
#115=CONTEXT_DEPENDENT_SHAPE_REPRESENTATION(#74,#10917);
#116=CONTEXT_DEPENDENT_SHAPE_REPRESENTATION(#75,#10918);
#117=CONTEXT_DEPENDENT_SHAPE_REPRESENTATION(#76,#10924);
#118=CONTEXT_DEPENDENT_SHAPE_REPRESENTATION(#77,#10925);
#119=CONTEXT_DEPENDENT_SHAPE_REPRESENTATION(#78,#10926);
#120=CONTEXT_DEPENDENT_SHAPE_REPRESENTATION(#79,#10927);
#121=CONTEXT_DEPENDENT_SHAPE_REPRESENTATION(#80,#10928);
#122=CONTEXT_DEPENDENT_SHAPE_REPRESENTATION(#81,#10929);
#123=CONTEXT_DEPENDENT_SHAPE_REPRESENTATION(#82,#10930);
#124=CONTEXT_DEPENDENT_SHAPE_REPRESENTATION(#83,#10931);
#125=CONTEXT_DEPENDENT_SHAPE_REPRESENTATION(#84,#10932);
#126=CONTEXT_DEPENDENT_SHAPE_REPRESENTATION(#85,#10933);
#127=CONTEXT_DEPENDENT_SHAPE_REPRESENTATION(#86,#10934);
#128=CONTEXT_DEPENDENT_SHAPE_REPRESENTATION(#87,#10935);
#129=CONTEXT_DEPENDENT_SHAPE_REPRESENTATION(#88,#10936);
#130=CONTEXT_DEPENDENT_SHAPE_REPRESENTATION(#89,#10937);
#131=CONTEXT_DEPENDENT_SHAPE_REPRESENTATION(#90,#10938);
#132=CONTEXT_DEPENDENT_SHAPE_REPRESENTATION(#91,#10939);
#133=CONTEXT_DEPENDENT_SHAPE_REPRESENTATION(#92,#10940);
#134=NEXT_ASSEMBLY_USAGE_OCCURRENCE('Inner ring:1','Inner ring:1',
'Inner ring:1',#10979,#10980,'Inner ring:1');
#135=NEXT_ASSEMBLY_USAGE_OCCURRENCE('Outer ring:1','Outer ring:1',
'Outer ring:1',#10979,#10981,'Outer ring:1');
#136=NEXT_ASSEMBLY_USAGE_OCCURRENCE('Balls:1','Balls:1','Balls:1',#10979,
#10982,'Balls:1');
#137=NEXT_ASSEMBLY_USAGE_OCCURRENCE('Cage:1','Cage:1','Cage:1',#10979,#10983,
'Cage:1');
#138=NEXT_ASSEMBLY_USAGE_OCCURRENCE('Seals 2RS:1','Seals 2RS:1',
'Seals 2RS:1',#10979,#10984,'Seals 2RS:1');
#139=NEXT_ASSEMBLY_USAGE_OCCURRENCE('Demonstrator base plate:1',
'Demonstrator base plate:1','Demonstrator base plate:1',#10972,#10973,
'Demonstrator base plate:1');
#140=NEXT_ASSEMBLY_USAGE_OCCURRENCE('Foot strip:1','Foot strip:1',
'Foot strip:1',#10972,#10974,'Foot strip:1');
#141=NEXT_ASSEMBLY_USAGE_OCCURRENCE('Foot strip (1):1',
'Foot strip (1):1','Foot strip (1):1',#10972,#10975,'Foot strip (1):1');
#142=NEXT_ASSEMBLY_USAGE_OCCURRENCE('Bearing cap:1','Bearing cap:1',
'Bearing cap:1',#10972,#10976,'Bearing cap:1');
#143=NEXT_ASSEMBLY_USAGE_OCCURRENCE('Bearing cap (1):1',
'Bearing cap (1):1','Bearing cap (1):1',#10972,#10977,
'Bearing cap (1):1');
#144=NEXT_ASSEMBLY_USAGE_OCCURRENCE('Cap Screw - M5x20:2',
'Cap Screw - M5x20:2','Cap Screw - M5x20:2',#10972,#10978,
'Cap Screw - M5x20:2');
#145=NEXT_ASSEMBLY_USAGE_OCCURRENCE('Cap Screw - M5x20:3',
'Cap Screw - M5x20:3','Cap Screw - M5x20:3',#10972,#10978,
'Cap Screw - M5x20:3');
#146=NEXT_ASSEMBLY_USAGE_OCCURRENCE('Cap Screw - M5x20:4',
'Cap Screw - M5x20:4','Cap Screw - M5x20:4',#10972,#10978,
'Cap Screw - M5x20:4');
#147=NEXT_ASSEMBLY_USAGE_OCCURRENCE('Cap Screw - M5x20:5',
'Cap Screw - M5x20:5','Cap Screw - M5x20:5',#10972,#10978,
'Cap Screw - M5x20:5');
#148=NEXT_ASSEMBLY_USAGE_OCCURRENCE(
'Sealed Ball Bearing - 10 x 30 x 9 mm:2',
'Sealed Ball Bearing - 10 x 30 x 9 mm:2',
'Sealed Ball Bearing - 10 x 30 x 9 mm:2',#10972,#10979,
'Sealed Ball Bearing - 10 x 30 x 9 mm:2');
#149=NEXT_ASSEMBLY_USAGE_OCCURRENCE('M4x10 Cap Screw:2',
'M4x10 Cap Screw:2','M4x10 Cap Screw:2',#10972,#10994,
'M4x10 Cap Screw:2');
#150=NEXT_ASSEMBLY_USAGE_OCCURRENCE('M4x10 Cap Screw:3',
'M4x10 Cap Screw:3','M4x10 Cap Screw:3',#10972,#10994,
'M4x10 Cap Screw:3');
#151=NEXT_ASSEMBLY_USAGE_OCCURRENCE('M4x10 Cap Screw:4',
'M4x10 Cap Screw:4','M4x10 Cap Screw:4',#10972,#10994,
'M4x10 Cap Screw:4');
#152=NEXT_ASSEMBLY_USAGE_OCCURRENCE('M4x10 Cap Screw:5',
'M4x10 Cap Screw:5','M4x10 Cap Screw:5',#10972,#10994,
'M4x10 Cap Screw:5');
#153=NEXT_ASSEMBLY_USAGE_OCCURRENCE(
'Sealed Ball Bearing - 10 x 30 x 9 mm:3',
'Sealed Ball Bearing - 10 x 30 x 9 mm:3',
'Sealed Ball Bearing - 10 x 30 x 9 mm:3',#10972,#10979,
'Sealed Ball Bearing - 10 x 30 x 9 mm:3');
#154=NEXT_ASSEMBLY_USAGE_OCCURRENCE('M4x10 Cap Screw:7',
'M4x10 Cap Screw:7','M4x10 Cap Screw:7',#10972,#10994,
'M4x10 Cap Screw:7');
#155=NEXT_ASSEMBLY_USAGE_OCCURRENCE('M4x10 Cap Screw:8',
'M4x10 Cap Screw:8','M4x10 Cap Screw:8',#10972,#10994,
'M4x10 Cap Screw:8');
#156=NEXT_ASSEMBLY_USAGE_OCCURRENCE('M4x10 Cap Screw:9',
'M4x10 Cap Screw:9','M4x10 Cap Screw:9',#10972,#10994,
'M4x10 Cap Screw:9');
#157=NEXT_ASSEMBLY_USAGE_OCCURRENCE('M4x10 Cap Screw:10',
'M4x10 Cap Screw:10','M4x10 Cap Screw:10',#10972,#10994,
'M4x10 Cap Screw:10');
#158=NEXT_ASSEMBLY_USAGE_OCCURRENCE('Input crank and spindle:1',
'Input crank and spindle:1','Input crank and spindle:1',#10985,#10986,
'Input crank and spindle:1');
#159=NEXT_ASSEMBLY_USAGE_OCCURRENCE('Lower bearing sleeve:1',
'Lower bearing sleeve:1','Lower bearing sleeve:1',#10985,#10987,
'Lower bearing sleeve:1');
#160=NEXT_ASSEMBLY_USAGE_OCCURRENCE('Retaining collar:1',
'Retaining collar:1','Retaining collar:1',#10985,#10988,
'Retaining collar:1');
#161=NEXT_ASSEMBLY_USAGE_OCCURRENCE('Drive pin:1','Drive pin:1',
'Drive pin:1',#10985,#10989,'Drive pin:1');
#162=NEXT_ASSEMBLY_USAGE_OCCURRENCE('Locking cam:1','Locking cam:1',
'Locking cam:1',#10985,#10990,'Locking cam:1');
#163=NEXT_ASSEMBLY_USAGE_OCCURRENCE('Locking cam spacer:1',
'Locking cam spacer:1','Locking cam spacer:1',#10985,#10991,
'Locking cam spacer:1');
#164=NEXT_ASSEMBLY_USAGE_OCCURRENCE('Cam keeper:1','Cam keeper:1',
'Cam keeper:1',#10985,#10992,'Cam keeper:1');
#165=NEXT_ASSEMBLY_USAGE_OCCURRENCE('Crank grip:1','Crank grip:1',
'Crank grip:1',#10985,#10993,'Crank grip:1');
#166=NEXT_ASSEMBLY_USAGE_OCCURRENCE('M4x4 collar screw:2',
'M4x4 collar screw:2','M4x4 collar screw:2',#10985,#10999,
'M4x4 collar screw:2');
#167=NEXT_ASSEMBLY_USAGE_OCCURRENCE('M4x10 Cap Screw:6',
'M4x10 Cap Screw:6','M4x10 Cap Screw:6',#10985,#10994,
'M4x10 Cap Screw:6');
#168=NEXT_ASSEMBLY_USAGE_OCCURRENCE('Output wheel and spindle:1',
'Output wheel and spindle:1','Output wheel and spindle:1',#10995,#10996,
'Output wheel and spindle:1');
#169=NEXT_ASSEMBLY_USAGE_OCCURRENCE('Lower bearing sleeve (1):1',
'Lower bearing sleeve (1):1','Lower bearing sleeve (1):1',#10995,#10997,
'Lower bearing sleeve (1):1');
#170=NEXT_ASSEMBLY_USAGE_OCCURRENCE('Retaining collar (1):1',
'Retaining collar (1):1','Retaining collar (1):1',#10995,#10998,
'Retaining collar (1):1');
#171=NEXT_ASSEMBLY_USAGE_OCCURRENCE('M4x4 collar screw:3',
'M4x4 collar screw:3','M4x4 collar screw:3',#10995,#10999,
'M4x4 collar screw:3');
#172=NEXT_ASSEMBLY_USAGE_OCCURRENCE('Bearing base:1','Bearing base:1',
'Bearing base:1',#10971,#10972,'Bearing base:1');
#173=NEXT_ASSEMBLY_USAGE_OCCURRENCE('Input crank and locking cam:1',
'Input crank and locking cam:1','Input crank and locking cam:1',#10971,
#10985,'Input crank and locking cam:1');
#174=NEXT_ASSEMBLY_USAGE_OCCURRENCE('Four-slot output wheel:1',
'Four-slot output wheel:1','Four-slot output wheel:1',#10971,#10995,
'Four-slot output wheel:1');
#175=SPHERICAL_SURFACE('',#6230,0.23815);
#176=SPHERICAL_SURFACE('',#6232,0.23815);
#177=SPHERICAL_SURFACE('',#6234,0.23815);
#178=SPHERICAL_SURFACE('',#6236,0.23815);
#179=SPHERICAL_SURFACE('',#6238,0.23815);
#180=SPHERICAL_SURFACE('',#6240,0.23815);
#181=SPHERICAL_SURFACE('',#6242,0.23815);
#182=SPHERICAL_SURFACE('',#6244,0.23815);
#183=SPHERICAL_SURFACE('',#6247,0.247676);
#184=SPHERICAL_SURFACE('',#6263,0.247676);
#185=SPHERICAL_SURFACE('',#6268,0.247676);
#186=SPHERICAL_SURFACE('',#6273,0.247676);
#187=SPHERICAL_SURFACE('',#6278,0.247676);
#188=SPHERICAL_SURFACE('',#6283,0.247676);
#189=SPHERICAL_SURFACE('',#6288,0.247676);
#190=SPHERICAL_SURFACE('',#6296,0.247676);
#191=TOROIDAL_SURFACE('',#6190,1.,0.247676);
#192=TOROIDAL_SURFACE('',#6210,1.,0.247676);
#193=ORIENTED_CLOSED_SHELL('',*,#5635,.F.);
#194=ORIENTED_CLOSED_SHELL('',*,#5657,.F.);
#195=CONICAL_SURFACE('',#6165,0.4,0.785398163397448);
#196=CONICAL_SURFACE('',#6169,0.41,0.785398163397448);
#197=CONICAL_SURFACE('',#6173,0.26,0.463647609000806);
#198=CONICAL_SURFACE('',#6177,0.225,0.785398163397448);
#199=CONICAL_SURFACE('',#6201,0.53,0.785398163397448);
#200=CONICAL_SURFACE('',#6208,0.53,0.785398163397448);
#201=CONICAL_SURFACE('',#6221,1.47,0.785398163397449);
#202=CONICAL_SURFACE('',#6225,1.47,0.785398163397449);
#203=CONICAL_SURFACE('',#6456,0.325,0.785398163397448);
#204=CONICAL_SURFACE('',#6460,0.335,0.785398163397448);
#205=CONICAL_SURFACE('',#6464,0.21,0.463647609000806);
#206=CONICAL_SURFACE('',#6646,0.185,0.785398163397449);
#207=BREP_WITH_VOIDS('Body1',#5634,(#193));
#208=BREP_WITH_VOIDS('Body1',#5658,(#194));
#209=SHAPE_REPRESENTATION_RELATIONSHIP('SRR','None',#10943,#233);
#210=SHAPE_REPRESENTATION_RELATIONSHIP('SRR','None',#10944,#234);
#211=SHAPE_REPRESENTATION_RELATIONSHIP('SRR','None',#10945,#235);
#212=SHAPE_REPRESENTATION_RELATIONSHIP('SRR','None',#10946,#236);
#213=SHAPE_REPRESENTATION_RELATIONSHIP('SRR','None',#10947,#237);
#214=SHAPE_REPRESENTATION_RELATIONSHIP('SRR','None',#10948,#238);
#215=SHAPE_REPRESENTATION_RELATIONSHIP('SRR','None',#10950,#239);
#216=SHAPE_REPRESENTATION_RELATIONSHIP('SRR','None',#10951,#240);
#217=SHAPE_REPRESENTATION_RELATIONSHIP('SRR','None',#10952,#241);
#218=SHAPE_REPRESENTATION_RELATIONSHIP('SRR','None',#10953,#242);
#219=SHAPE_REPRESENTATION_RELATIONSHIP('SRR','None',#10954,#243);
#220=SHAPE_REPRESENTATION_RELATIONSHIP('SRR','None',#10956,#244);
#221=SHAPE_REPRESENTATION_RELATIONSHIP('SRR','None',#10957,#245);
#222=SHAPE_REPRESENTATION_RELATIONSHIP('SRR','None',#10958,#246);
#223=SHAPE_REPRESENTATION_RELATIONSHIP('SRR','None',#10959,#247);
#224=SHAPE_REPRESENTATION_RELATIONSHIP('SRR','None',#10960,#248);
#225=SHAPE_REPRESENTATION_RELATIONSHIP('SRR','None',#10961,#249);
#226=SHAPE_REPRESENTATION_RELATIONSHIP('SRR','None',#10962,#250);
#227=SHAPE_REPRESENTATION_RELATIONSHIP('SRR','None',#10963,#251);
#228=SHAPE_REPRESENTATION_RELATIONSHIP('SRR','None',#10964,#252);
#229=SHAPE_REPRESENTATION_RELATIONSHIP('SRR','None',#10966,#253);
#230=SHAPE_REPRESENTATION_RELATIONSHIP('SRR','None',#10967,#254);
#231=SHAPE_REPRESENTATION_RELATIONSHIP('SRR','None',#10968,#255);
#232=SHAPE_REPRESENTATION_RELATIONSHIP('SRR','None',#10969,#256);
#233=ADVANCED_BREP_SHAPE_REPRESENTATION('',(#289),#10810);
#234=ADVANCED_BREP_SHAPE_REPRESENTATION('',(#290),#10811);
#235=ADVANCED_BREP_SHAPE_REPRESENTATION('',(#291),#10812);
#236=ADVANCED_BREP_SHAPE_REPRESENTATION('',(#292),#10813);
#237=ADVANCED_BREP_SHAPE_REPRESENTATION('',(#293),#10814);
#238=ADVANCED_BREP_SHAPE_REPRESENTATION('',(#207),#10815);
#239=ADVANCED_BREP_SHAPE_REPRESENTATION('',(#294),#10817);
#240=ADVANCED_BREP_SHAPE_REPRESENTATION('',(#295),#10818);
#241=ADVANCED_BREP_SHAPE_REPRESENTATION('',(#296,#297,#298,#299,#300,#301,
#302,#303),#10819);
#242=ADVANCED_BREP_SHAPE_REPRESENTATION('',(#304),#10820);
#243=ADVANCED_BREP_SHAPE_REPRESENTATION('',(#305,#306),#10821);
#244=ADVANCED_BREP_SHAPE_REPRESENTATION('',(#307),#10823);
#245=ADVANCED_BREP_SHAPE_REPRESENTATION('',(#308),#10824);
#246=ADVANCED_BREP_SHAPE_REPRESENTATION('',(#309),#10825);
#247=ADVANCED_BREP_SHAPE_REPRESENTATION('',(#310),#10826);
#248=ADVANCED_BREP_SHAPE_REPRESENTATION('',(#311),#10827);
#249=ADVANCED_BREP_SHAPE_REPRESENTATION('',(#312),#10828);
#250=ADVANCED_BREP_SHAPE_REPRESENTATION('',(#313),#10829);
#251=ADVANCED_BREP_SHAPE_REPRESENTATION('',(#314),#10830);
#252=ADVANCED_BREP_SHAPE_REPRESENTATION('',(#208),#10831);
#253=ADVANCED_BREP_SHAPE_REPRESENTATION('',(#315),#10833);
#254=ADVANCED_BREP_SHAPE_REPRESENTATION('',(#316),#10834);
#255=ADVANCED_BREP_SHAPE_REPRESENTATION('',(#317),#10835);
#256=ADVANCED_BREP_SHAPE_REPRESENTATION('',(#318),#10836);
#257=STYLED_ITEM('',(#11145),#289);
#258=STYLED_ITEM('',(#11152),#290);
#259=STYLED_ITEM('',(#11152),#291);
#260=STYLED_ITEM('',(#11166),#292);
#261=STYLED_ITEM('',(#11166),#293);
#262=STYLED_ITEM('',(#11173),#207);
#263=STYLED_ITEM('',(#11166),#294);
#264=STYLED_ITEM('',(#11166),#295);
#265=STYLED_ITEM('',(#11166),#296);
#266=STYLED_ITEM('',(#11166),#297);
#267=STYLED_ITEM('',(#11166),#298);
#268=STYLED_ITEM('',(#11166),#299);
#269=STYLED_ITEM('',(#11166),#300);
#270=STYLED_ITEM('',(#11166),#301);
#271=STYLED_ITEM('',(#11166),#302);
#272=STYLED_ITEM('',(#11166),#303);
#273=STYLED_ITEM('',(#11166),#304);
#274=STYLED_ITEM('',(#11166),#305);
#275=STYLED_ITEM('',(#11166),#306);
#276=STYLED_ITEM('',(#11159),#307);
#277=STYLED_ITEM('',(#11166),#308);
#278=STYLED_ITEM('',(#11180),#309);
#279=STYLED_ITEM('',(#11166),#310);
#280=STYLED_ITEM('',(#11159),#311);
#281=STYLED_ITEM('',(#11180),#312);
#282=STYLED_ITEM('',(#11152),#313);
#283=STYLED_ITEM('',(#11173),#314);
#284=STYLED_ITEM('',(#11173),#208);
#285=STYLED_ITEM('',(#11159),#315);
#286=STYLED_ITEM('',(#11166),#316);
#287=STYLED_ITEM('',(#11180),#317);
#288=STYLED_ITEM('',(#11173),#318);
#289=MANIFOLD_SOLID_BREP('Body1',#5629);
#290=MANIFOLD_SOLID_BREP('Body1',#5630);
#291=MANIFOLD_SOLID_BREP('Body1',#5631);
#292=MANIFOLD_SOLID_BREP('Body1',#5632);
#293=MANIFOLD_SOLID_BREP('Body1',#5633);
#294=MANIFOLD_SOLID_BREP('Body1',#5636);
#295=MANIFOLD_SOLID_BREP('Body1',#5637);
#296=MANIFOLD_SOLID_BREP('Body1',#5638);
#297=MANIFOLD_SOLID_BREP('Body2',#5639);
#298=MANIFOLD_SOLID_BREP('Body3',#5640);
#299=MANIFOLD_SOLID_BREP('Body4',#5641);
#300=MANIFOLD_SOLID_BREP('Body5',#5642);
#301=MANIFOLD_SOLID_BREP('Body6',#5643);
#302=MANIFOLD_SOLID_BREP('Body7',#5644);
#303=MANIFOLD_SOLID_BREP('Body8',#5645);
#304=MANIFOLD_SOLID_BREP('Continuous crown cage',#5646);
#305=MANIFOLD_SOLID_BREP('Body1',#5647);
#306=MANIFOLD_SOLID_BREP('Body2',#5648);
#307=MANIFOLD_SOLID_BREP('Body1',#5649);
#308=MANIFOLD_SOLID_BREP('Body1',#5650);
#309=MANIFOLD_SOLID_BREP('Body1',#5651);
#310=MANIFOLD_SOLID_BREP('Body1',#5652);
#311=MANIFOLD_SOLID_BREP('Body1',#5653);
#312=MANIFOLD_SOLID_BREP('Body1',#5654);
#313=MANIFOLD_SOLID_BREP('Body1',#5655);
#314=MANIFOLD_SOLID_BREP('Body1',#5656);
#315=MANIFOLD_SOLID_BREP('Body1',#5659);
#316=MANIFOLD_SOLID_BREP('Body1',#5660);
#317=MANIFOLD_SOLID_BREP('Body1',#5661);
#318=MANIFOLD_SOLID_BREP('Body1',#5662);
#319=B_SPLINE_CURVE_WITH_KNOTS('',3,(#8545,#8546,#8547,#8548,#8549,#8550,
#8551,#8552,#8553,#8554,#8555,#8556,#8557,#8558,#8559,#8560,#8561,#8562,
#8563,#8564,#8565,#8566,#8567,#8568,#8569,#8570,#8571,#8572,#8573,#8574,
#8575,#8576,#8577,#8578),.UNSPECIFIED.,.T.,.F.,(4,2,2,2,2,2,2,2,2,2,2,2,
2,2,2,2,4),(0.,0.094594182476448,0.189188364952896,0.283770357603024,0.378352350253152,
0.472934342903279,0.567516335553407,0.662110518029855,0.756704700506303,
0.851298882982751,0.945893065459199,1.04047505810933,1.13505705075945,1.22963904340958,
1.32422103605971,1.41881521853616,1.51340940101261),.UNSPECIFIED.);
#320=B_SPLINE_CURVE_WITH_KNOTS('',3,(#8621,#8622,#8623,#8624,#8625,#8626,
#8627,#8628,#8629,#8630,#8631,#8632,#8633,#8634,#8635,#8636,#8637,#8638,
#8639,#8640,#8641,#8642,#8643,#8644,#8645,#8646,#8647,#8648,#8649,#8650,
#8651,#8652,#8653,#8654),.UNSPECIFIED.,.T.,.F.,(4,2,2,2,2,2,2,2,2,2,2,2,
2,2,2,2,4),(0.,0.0945941824764479,0.189188364952896,0.283770357603024,0.378352350253152,
0.47293434290328,0.567516335553408,0.662110518029856,0.756704700506303,
0.851298882982751,0.945893065459199,1.04047505810933,1.13505705075946,1.22963904340958,
1.32422103605971,1.41881521853616,1.51340940101261),.UNSPECIFIED.);
#321=B_SPLINE_CURVE_WITH_KNOTS('',3,(#9240,#9241,#9242,#9243,#9244,#9245,
#9246,#9247,#9248,#9249,#9250,#9251,#9252,#9253,#9254,#9255,#9256,#9257,
#9258,#9259,#9260,#9261),.UNSPECIFIED.,.F.,.F.,(4,2,2,2,2,2,2,2,2,2,4),
(0.0473477652366656,0.126350602536658,0.189525903804987,0.252701205073317,
0.313298422430275,0.373895639787233,0.434492857144191,0.495090074501149,
0.558265375769478,0.621440677037807,0.7004435143378),.UNSPECIFIED.);
#322=B_SPLINE_CURVE_WITH_KNOTS('',3,(#9265,#9266,#9267,#9268,#9269,#9270,
#9271,#9272,#9273,#9274,#9275,#9276,#9277,#9278,#9279,#9280,#9281,#9282,
#9283,#9284,#9285,#9286),.UNSPECIFIED.,.F.,.F.,(4,2,2,2,2,2,2,2,2,2,4),
(0.0464897534940957,0.0852567806515119,0.170513561303024,0.246687263103517,
0.308657850341199,0.370628437578881,0.432599024816563,0.494569612054245,
0.570743313854739,0.656000094506251,0.694767121663666),.UNSPECIFIED.);
#323=B_SPLINE_CURVE_WITH_KNOTS('',3,(#9292,#9293,#9294,#9295,#9296,#9297,
#9298,#9299,#9300,#9301,#9302,#9303,#9304,#9305,#9306,#9307,#9308,#9309,
#9310,#9311,#9312,#9313),.UNSPECIFIED.,.F.,.F.,(4,2,2,2,2,2,2,2,2,2,4),
(0.0464897534940957,0.0852567806515118,0.170513561303024,0.246687263103517,
0.308657850341199,0.370628437578881,0.432599024816563,0.494569612054245,
0.570743313854738,0.65600009450625,0.694767121663666),.UNSPECIFIED.);
#324=B_SPLINE_CURVE_WITH_KNOTS('',3,(#9317,#9318,#9319,#9320,#9321,#9322,
#9323,#9324,#9325,#9326,#9327,#9328,#9329,#9330,#9331,#9332,#9333,#9334,
#9335,#9336,#9337,#9338),.UNSPECIFIED.,.F.,.F.,(4,2,2,2,2,2,2,2,2,2,4),
(0.0464897534940957,0.0852567806515119,0.170513561303024,0.246687263103517,
0.308657850341199,0.370628437578881,0.432599024816563,0.494569612054245,
0.570743313854739,0.656000094506251,0.694767121663666),.UNSPECIFIED.);
#325=B_SPLINE_CURVE_WITH_KNOTS('',3,(#9342,#9343,#9344,#9345,#9346,#9347,
#9348,#9349,#9350,#9351,#9352,#9353),.UNSPECIFIED.,.F.,.F.,(4,2,2,2,2,4),
(0.0464897534940957,0.0852567806515119,0.170513561303024,0.246687263103517,
0.308657850341199,0.370628437578881),.UNSPECIFIED.);
#326=B_SPLINE_CURVE_WITH_KNOTS('',3,(#9358,#9359,#9360,#9361,#9362,#9363,
#9364,#9365,#9366,#9367,#9368,#9369),.UNSPECIFIED.,.F.,.F.,(4,2,2,2,2,4),
(0.370628437578881,0.432599024816563,0.494569612054245,0.570743313854738,
0.65600009450625,0.694767121663666),.UNSPECIFIED.);
#327=B_SPLINE_CURVE_WITH_KNOTS('',3,(#9373,#9374,#9375,#9376,#9377,#9378,
#9379,#9380,#9381,#9382,#9383,#9384,#9385,#9386,#9387,#9388,#9389,#9390,
#9391,#9392,#9393,#9394),.UNSPECIFIED.,.F.,.F.,(4,2,2,2,2,2,2,2,2,2,4),
(0.0464897534940957,0.0852567806515121,0.170513561303024,0.246687263103518,
0.308657850341199,0.370628437578881,0.432599024816563,0.494569612054245,
0.570743313854738,0.65600009450625,0.694767121663666),.UNSPECIFIED.);
#328=B_SPLINE_CURVE_WITH_KNOTS('',3,(#9398,#9399,#9400,#9401,#9402,#9403,
#9404,#9405,#9406,#9407,#9408,#9409,#9410,#9411,#9412,#9413,#9414,#9415,
#9416,#9417,#9418,#9419),.UNSPECIFIED.,.F.,.F.,(4,2,2,2,2,2,2,2,2,2,4),
(0.0464897534940957,0.0852567806515119,0.170513561303024,0.246687263103517,
0.308657850341199,0.370628437578881,0.432599024816563,0.494569612054245,
0.570743313854738,0.65600009450625,0.694767121663667),.UNSPECIFIED.);
#329=B_SPLINE_CURVE_WITH_KNOTS('',3,(#9423,#9424,#9425,#9426,#9427,#9428,
#9429,#9430,#9431,#9432,#9433,#9434,#9435,#9436,#9437,#9438,#9439,#9440,
#9441,#9442,#9443,#9444),.UNSPECIFIED.,.F.,.F.,(4,2,2,2,2,2,2,2,2,2,4),
(0.0464897534940957,0.0852567806515119,0.170513561303024,0.246687263103517,
0.308657850341199,0.370628437578881,0.432599024816563,0.494569612054245,
0.570743313854738,0.65600009450625,0.694767121663666),.UNSPECIFIED.);
#330=B_SPLINE_CURVE_WITH_KNOTS('',3,(#9448,#9449,#9450,#9451,#9452,#9453,
#9454,#9455,#9456,#9457,#9458,#9459,#9460,#9461,#9462,#9463,#9464,#9465,
#9466,#9467,#9468,#9469),.UNSPECIFIED.,.F.,.F.,(4,2,2,2,2,2,2,2,2,2,4),
(0.0464897534940957,0.0852567806515119,0.170513561303024,0.246687263103517,
0.308657850341199,0.370628437578881,0.432599024816563,0.494569612054245,
0.570743313854739,0.656000094506251,0.694767121663667),.UNSPECIFIED.);
#331=B_SPLINE_CURVE_WITH_KNOTS('',3,(#9477,#9478,#9479,#9480,#9481,#9482,
#9483,#9484,#9485,#9486,#9487,#9488,#9489,#9490,#9491,#9492,#9493,#9494,
#9495,#9496,#9497,#9498),.UNSPECIFIED.,.F.,.F.,(4,2,2,2,2,2,2,2,2,2,4),
(0.0473477652366656,0.126350602536658,0.189525903804987,0.252701205073316,
0.313298422430274,0.373895639787232,0.434492857144191,0.495090074501149,
0.558265375769478,0.621440677037807,0.7004435143378),.UNSPECIFIED.);
#332=B_SPLINE_CURVE_WITH_KNOTS('',3,(#9506,#9507,#9508,#9509,#9510,#9511,
#9512,#9513,#9514,#9515,#9516,#9517,#9518,#9519,#9520,#9521,#9522,#9523,
#9524,#9525,#9526,#9527),.UNSPECIFIED.,.F.,.F.,(4,2,2,2,2,2,2,2,2,2,4),
(0.0473477652366656,0.126350602536658,0.189525903804987,0.252701205073317,
0.313298422430275,0.373895639787233,0.434492857144191,0.495090074501149,
0.558265375769478,0.621440677037807,0.7004435143378),.UNSPECIFIED.);
#333=B_SPLINE_CURVE_WITH_KNOTS('',3,(#9536,#9537,#9538,#9539,#9540,#9541,
#9542,#9543,#9544,#9545,#9546,#9547),.UNSPECIFIED.,.F.,.F.,(4,2,2,2,2,4),
(0.0473477652366656,0.126350602536658,0.189525903804987,0.252701205073316,
0.313298422430275,0.373895639787233),.UNSPECIFIED.);
#334=B_SPLINE_CURVE_WITH_KNOTS('',3,(#9549,#9550,#9551,#9552,#9553,#9554,
#9555,#9556,#9557,#9558,#9559,#9560),.UNSPECIFIED.,.F.,.F.,(4,2,2,2,2,4),
(0.373895639787233,0.434492857144191,0.495090074501149,0.558265375769478,
0.621440677037807,0.7004435143378),.UNSPECIFIED.);
#335=B_SPLINE_CURVE_WITH_KNOTS('',3,(#9567,#9568,#9569,#9570,#9571,#9572,
#9573,#9574,#9575,#9576,#9577,#9578,#9579,#9580,#9581,#9582,#9583,#9584,
#9585,#9586,#9587,#9588),.UNSPECIFIED.,.F.,.F.,(4,2,2,2,2,2,2,2,2,2,4),
(0.0473477652366656,0.126350602536658,0.189525903804987,0.252701205073316,
0.313298422430275,0.373895639787233,0.434492857144191,0.495090074501149,
0.558265375769478,0.621440677037807,0.7004435143378),.UNSPECIFIED.);
#336=B_SPLINE_CURVE_WITH_KNOTS('',3,(#9596,#9597,#9598,#9599,#9600,#9601,
#9602,#9603,#9604,#9605,#9606,#9607,#9608,#9609,#9610,#9611,#9612,#9613,
#9614,#9615,#9616,#9617),.UNSPECIFIED.,.F.,.F.,(4,2,2,2,2,2,2,2,2,2,4),
(0.0473477652366656,0.126350602536658,0.189525903804987,0.252701205073317,
0.313298422430275,0.373895639787233,0.434492857144191,0.495090074501149,
0.558265375769478,0.621440677037807,0.7004435143378),.UNSPECIFIED.);
#337=B_SPLINE_CURVE_WITH_KNOTS('',3,(#9625,#9626,#9627,#9628,#9629,#9630,
#9631,#9632,#9633,#9634,#9635,#9636,#9637,#9638,#9639,#9640,#9641,#9642,
#9643,#9644,#9645,#9646),.UNSPECIFIED.,.F.,.F.,(4,2,2,2,2,2,2,2,2,2,4),
(0.0473477652366656,0.126350602536658,0.189525903804987,0.252701205073316,
0.313298422430275,0.373895639787233,0.434492857144191,0.495090074501149,
0.558265375769478,0.621440677037807,0.7004435143378),.UNSPECIFIED.);
#338=B_SPLINE_CURVE_WITH_KNOTS('',3,(#9655,#9656,#9657,#9658,#9659,#9660,
#9661,#9662,#9663,#9664,#9665,#9666,#9667,#9668,#9669,#9670,#9671,#9672,
#9673,#9674,#9675,#9676),.UNSPECIFIED.,.F.,.F.,(4,2,2,2,2,2,2,2,2,2,4),
(0.0473477652366656,0.126350602536658,0.189525903804987,0.252701205073317,
0.313298422430275,0.373895639787233,0.434492857144191,0.495090074501149,
0.558265375769478,0.621440677037807,0.7004435143378),.UNSPECIFIED.);
#339=B_SPLINE_CURVE_WITH_KNOTS('',3,(#9829,#9830,#9831,#9832,#9833,#9834,
#9835,#9836,#9837,#9838,#9839,#9840,#9841,#9842,#9843,#9844,#9845,#9846,
#9847,#9848,#9849,#9850,#9851,#9852,#9853,#9854,#9855,#9856,#9857,#9858,
#9859,#9860,#9861,#9862),.UNSPECIFIED.,.T.,.F.,(4,2,2,2,2,2,2,2,2,2,2,2,
2,2,2,2,4),(0.,0.0623062782223143,0.124612556444629,0.186916384615149,0.249220212785669,
0.31152404095619,0.37382786912671,0.436134147349024,0.498440425571339,0.560746703793653,
0.623052982015967,0.685356810186488,0.747660638357008,0.809964466527529,
0.872268294698049,0.934574572920363,0.996880851142677),.UNSPECIFIED.);
#340=B_SPLINE_CURVE_WITH_KNOTS('',3,(#9865,#9866,#9867,#9868,#9869,#9870,
#9871,#9872,#9873,#9874,#9875,#9876,#9877,#9878),.UNSPECIFIED.,.F.,.F.,
(4,2,2,2,2,2,4),(0.618551524396292,0.626563103102765,0.689203386094988,
0.751843669087211,0.814483952079434,0.877124235071657,0.88513581377813),
 .UNSPECIFIED.);
#341=B_SPLINE_CURVE_WITH_KNOTS('',3,(#9881,#9882,#9883,#9884,#9885,#9886,
#9887,#9888,#9889,#9890,#9891,#9892,#9893,#9894),.UNSPECIFIED.,.F.,.F.,
(4,2,2,2,2,2,4),(0.117322411671485,0.125333990377958,0.187974273370181,
0.250614556362404,0.313254839354627,0.37589512234685,0.383906701053323),
 .UNSPECIFIED.);
#342=B_SPLINE_CURVE_WITH_KNOTS('',3,(#9905,#9906,#9907,#9908,#9909,#9910,
#9911,#9912,#9913,#9914),.UNSPECIFIED.,.F.,.F.,(4,2,2,2,4),(0.,0.0623062782223142,
0.124612556444628,0.186916384615149,0.249220212785669),.UNSPECIFIED.);
#343=B_SPLINE_CURVE_WITH_KNOTS('',3,(#9916,#9917,#9918,#9919,#9920,#9921,
#9922,#9923,#9924,#9925),.UNSPECIFIED.,.F.,.F.,(4,2,2,2,4),(0.747660638357008,
0.809964466527529,0.872268294698049,0.934574572920363,0.996880851142677),
 .UNSPECIFIED.);
#344=B_SPLINE_CURVE_WITH_KNOTS('',3,(#9926,#9927,#9928,#9929,#9930,#9931,
#9932,#9933,#9934,#9935,#9936,#9937,#9938,#9939,#9940,#9941,#9942,#9943),
 .UNSPECIFIED.,.F.,.F.,(4,2,2,2,2,2,2,2,4),(0.249220212785669,0.31152404095619,
0.37382786912671,0.436134147349024,0.498440425571339,0.560746703793653,
0.623052982015967,0.685356810186488,0.747660638357008),.UNSPECIFIED.);
#345=B_SPLINE_CURVE_WITH_KNOTS('',3,(#9947,#9948,#9949,#9950,#9951,#9952,
#9953,#9954),.UNSPECIFIED.,.F.,.F.,(4,2,2,4),(0.618551524396292,0.626563103102765,
0.689203386094988,0.751843669087211),.UNSPECIFIED.);
#346=B_SPLINE_CURVE_WITH_KNOTS('',3,(#9958,#9959,#9960,#9961,#9962,#9963,
#9964,#9965),.UNSPECIFIED.,.F.,.F.,(4,2,2,4),(0.250614556362404,0.313254839354627,
0.37589512234685,0.383906701053323),.UNSPECIFIED.);
#347=B_SPLINE_CURVE_WITH_KNOTS('',3,(#9966,#9967,#9968,#9969,#9970,#9971,
#9972,#9973),.UNSPECIFIED.,.F.,.F.,(4,2,2,4),(0.117322411671484,0.125333990377958,
0.187974273370181,0.250614556362404),.UNSPECIFIED.);
#348=B_SPLINE_CURVE_WITH_KNOTS('',3,(#9974,#9975,#9976,#9977,#9978,#9979,
#9980,#9981),.UNSPECIFIED.,.F.,.F.,(4,2,2,4),(0.751843669087211,0.814483952079434,
0.877124235071657,0.885135813778131),.UNSPECIFIED.);
#349=B_SPLINE_CURVE_WITH_KNOTS('',3,(#10540,#10541,#10542,#10543,#10544,
#10545,#10546,#10547,#10548,#10549,#10550,#10551,#10552,#10553,#10554,#10555,
#10556,#10557,#10558,#10559,#10560,#10561,#10562,#10563,#10564,#10565,#10566,
#10567,#10568,#10569,#10570,#10571,#10572,#10573),.UNSPECIFIED.,.T.,.F.,
(4,2,2,2,2,2,2,2,2,2,2,2,2,2,2,2,4),(0.,0.0623062782223143,0.124612556444629,
0.186916384615149,0.249220212785669,0.31152404095619,0.37382786912671,0.436134147349024,
0.498440425571339,0.560746703793653,0.623052982015967,0.685356810186488,
0.747660638357008,0.809964466527529,0.872268294698049,0.934574572920363,
0.996880851142678),.UNSPECIFIED.);
#350=B_SPLINE_CURVE_WITH_KNOTS('',3,(#10576,#10577,#10578,#10579,#10580,
#10581,#10582,#10583,#10584,#10585,#10586,#10587,#10588,#10589),
 .UNSPECIFIED.,.F.,.F.,(4,2,2,2,2,2,4),(0.618551524396292,0.626563103102765,
0.689203386094988,0.751843669087211,0.814483952079434,0.877124235071657,
0.88513581377813),.UNSPECIFIED.);
#351=B_SPLINE_CURVE_WITH_KNOTS('',3,(#10592,#10593,#10594,#10595,#10596,
#10597,#10598,#10599,#10600,#10601,#10602,#10603,#10604,#10605),
 .UNSPECIFIED.,.F.,.F.,(4,2,2,2,2,2,4),(0.117322411671484,0.125333990377958,
0.187974273370181,0.250614556362404,0.313254839354627,0.37589512234685,
0.383906701053322),.UNSPECIFIED.);
#352=B_SPLINE_CURVE_WITH_KNOTS('',3,(#10616,#10617,#10618,#10619,#10620,
#10621,#10622,#10623,#10624,#10625),.UNSPECIFIED.,.F.,.F.,(4,2,2,2,4),(0.,
0.0623062782223142,0.124612556444628,0.186916384615149,0.249220212785669),
 .UNSPECIFIED.);
#353=B_SPLINE_CURVE_WITH_KNOTS('',3,(#10627,#10628,#10629,#10630,#10631,
#10632,#10633,#10634,#10635,#10636),.UNSPECIFIED.,.F.,.F.,(4,2,2,2,4),(0.747660638357008,
0.809964466527528,0.872268294698049,0.934574572920363,0.996880851142677),
 .UNSPECIFIED.);
#354=B_SPLINE_CURVE_WITH_KNOTS('',3,(#10637,#10638,#10639,#10640,#10641,
#10642,#10643,#10644,#10645,#10646,#10647,#10648,#10649,#10650,#10651,#10652,
#10653,#10654),.UNSPECIFIED.,.F.,.F.,(4,2,2,2,2,2,2,2,4),(0.249220212785669,
0.31152404095619,0.37382786912671,0.436134147349024,0.498440425571339,0.560746703793653,
0.623052982015967,0.685356810186488,0.747660638357008),.UNSPECIFIED.);
#355=B_SPLINE_CURVE_WITH_KNOTS('',3,(#10658,#10659,#10660,#10661,#10662,
#10663,#10664,#10665),.UNSPECIFIED.,.F.,.F.,(4,2,2,4),(0.618551507245623,
0.626563103102765,0.689203386094988,0.751843669087211),.UNSPECIFIED.);
#356=B_SPLINE_CURVE_WITH_KNOTS('',3,(#10669,#10670,#10671,#10672,#10673,
#10674,#10675,#10676),.UNSPECIFIED.,.F.,.F.,(4,2,2,4),(0.250614556362404,
0.313254839354627,0.37589512234685,0.383906718203992),.UNSPECIFIED.);
#357=B_SPLINE_CURVE_WITH_KNOTS('',3,(#10677,#10678,#10679,#10680,#10681,
#10682,#10683,#10684),.UNSPECIFIED.,.F.,.F.,(4,2,2,4),(0.117322394520816,
0.125333990377958,0.187974273370181,0.250614556362404),.UNSPECIFIED.);
#358=B_SPLINE_CURVE_WITH_KNOTS('',3,(#10685,#10686,#10687,#10688,#10689,
#10690,#10691,#10692),.UNSPECIFIED.,.F.,.F.,(4,2,2,4),(0.751843669087211,
0.814483952079434,0.877124235071657,0.8851358309288),.UNSPECIFIED.);
#359=FACE_BOUND('',#996,.T.);
#360=FACE_BOUND('',#998,.T.);
#361=FACE_BOUND('',#1009,.T.);
#362=FACE_BOUND('',#1011,.T.);
#363=FACE_BOUND('',#1014,.T.);
#364=FACE_BOUND('',#1017,.T.);
#365=FACE_BOUND('',#1020,.T.);
#366=FACE_BOUND('',#1023,.T.);
#367=FACE_BOUND('',#1029,.T.);
#368=FACE_BOUND('',#1031,.T.);
#369=FACE_BOUND('',#1033,.T.);
#370=FACE_BOUND('',#1035,.T.);
#371=FACE_BOUND('',#1044,.T.);
#372=FACE_BOUND('',#1045,.T.);
#373=FACE_BOUND('',#1046,.T.);
#374=FACE_BOUND('',#1047,.T.);
#375=FACE_BOUND('',#1048,.T.);
#376=FACE_BOUND('',#1049,.T.);
#377=FACE_BOUND('',#1050,.T.);
#378=FACE_BOUND('',#1051,.T.);
#379=FACE_BOUND('',#1052,.T.);
#380=FACE_BOUND('',#1053,.T.);
#381=FACE_BOUND('',#1054,.T.);
#382=FACE_BOUND('',#1055,.T.);
#383=FACE_BOUND('',#1056,.T.);
#384=FACE_BOUND('',#1057,.T.);
#385=FACE_BOUND('',#1059,.T.);
#386=FACE_BOUND('',#1060,.T.);
#387=FACE_BOUND('',#1074,.T.);
#388=FACE_BOUND('',#1075,.T.);
#389=FACE_BOUND('',#1076,.T.);
#390=FACE_BOUND('',#1077,.T.);
#391=FACE_BOUND('',#1078,.T.);
#392=FACE_BOUND('',#1080,.T.);
#393=FACE_BOUND('',#1081,.T.);
#394=FACE_BOUND('',#1082,.T.);
#395=FACE_BOUND('',#1083,.T.);
#396=FACE_BOUND('',#1084,.T.);
#397=FACE_BOUND('',#1085,.T.);
#398=FACE_BOUND('',#1086,.T.);
#399=FACE_BOUND('',#1087,.T.);
#400=FACE_BOUND('',#1102,.T.);
#401=FACE_BOUND('',#1104,.T.);
#402=FACE_BOUND('',#1107,.T.);
#403=FACE_BOUND('',#1110,.T.);
#404=FACE_BOUND('',#1113,.T.);
#405=FACE_BOUND('',#1120,.T.);
#406=FACE_BOUND('',#1124,.T.);
#407=FACE_BOUND('',#1125,.T.);
#408=FACE_BOUND('',#1126,.T.);
#409=FACE_BOUND('',#1127,.T.);
#410=FACE_BOUND('',#1128,.T.);
#411=FACE_BOUND('',#1131,.T.);
#412=FACE_BOUND('',#1133,.T.);
#413=FACE_BOUND('',#1136,.T.);
#414=FACE_BOUND('',#1139,.T.);
#415=FACE_BOUND('',#1142,.T.);
#416=FACE_BOUND('',#1149,.T.);
#417=FACE_BOUND('',#1153,.T.);
#418=FACE_BOUND('',#1154,.T.);
#419=FACE_BOUND('',#1155,.T.);
#420=FACE_BOUND('',#1156,.T.);
#421=FACE_BOUND('',#1157,.T.);
#422=FACE_BOUND('',#1163,.T.);
#423=FACE_BOUND('',#1181,.T.);
#424=FACE_BOUND('',#1184,.T.);
#425=FACE_BOUND('',#1189,.T.);
#426=FACE_BOUND('',#1194,.T.);
#427=FACE_BOUND('',#1222,.T.);
#428=FACE_BOUND('',#1225,.T.);
#429=FACE_BOUND('',#1228,.T.);
#430=FACE_BOUND('',#1231,.T.);
#431=FACE_BOUND('',#1234,.T.);
#432=FACE_BOUND('',#1241,.T.);
#433=FACE_BOUND('',#1242,.T.);
#434=FACE_BOUND('',#1249,.T.);
#435=FACE_BOUND('',#1250,.T.);
#436=FACE_BOUND('',#1254,.T.);
#437=FACE_BOUND('',#1259,.T.);
#438=FACE_BOUND('',#1264,.T.);
#439=FACE_BOUND('',#1266,.T.);
#440=FACE_BOUND('',#1274,.T.);
#441=FACE_BOUND('',#1276,.T.);
#442=FACE_BOUND('',#1278,.T.);
#443=FACE_BOUND('',#1280,.T.);
#444=FACE_BOUND('',#1282,.T.);
#445=FACE_BOUND('',#1284,.T.);
#446=FACE_BOUND('',#1293,.T.);
#447=FACE_BOUND('',#1298,.T.);
#448=FACE_BOUND('',#1302,.T.);
#449=FACE_BOUND('',#1304,.T.);
#450=FACE_BOUND('',#1308,.T.);
#451=FACE_BOUND('',#1310,.T.);
#452=FACE_BOUND('',#1314,.T.);
#453=FACE_BOUND('',#1316,.T.);
#454=FACE_BOUND('',#1331,.T.);
#455=FACE_BOUND('',#1346,.T.);
#456=FACE_BOUND('',#1347,.T.);
#457=FACE_BOUND('',#1348,.T.);
#458=FACE_BOUND('',#1349,.T.);
#459=FACE_BOUND('',#1358,.T.);
#460=FACE_BOUND('',#1360,.T.);
#461=FACE_BOUND('',#1372,.T.);
#462=FACE_BOUND('',#1383,.T.);
#463=FACE_BOUND('',#1397,.T.);
#464=FACE_BOUND('',#1403,.T.);
#465=FACE_BOUND('',#1405,.T.);
#466=FACE_BOUND('',#1413,.T.);
#467=FACE_BOUND('',#1415,.T.);
#468=FACE_BOUND('',#1417,.T.);
#469=FACE_BOUND('',#1419,.T.);
#470=FACE_BOUND('',#1429,.T.);
#471=PLANE('',#5934);
#472=PLANE('',#5938);
#473=PLANE('',#5942);
#474=PLANE('',#5946);
#475=PLANE('',#5950);
#476=PLANE('',#5957);
#477=PLANE('',#5961);
#478=PLANE('',#5965);
#479=PLANE('',#5969);
#480=PLANE('',#5973);
#481=PLANE('',#5980);
#482=PLANE('',#5985);
#483=PLANE('',#5990);
#484=PLANE('',#5995);
#485=PLANE('',#6005);
#486=PLANE('',#6007);
#487=PLANE('',#6009);
#488=PLANE('',#6011);
#489=PLANE('',#6013);
#490=PLANE('',#6014);
#491=PLANE('',#6015);
#492=PLANE('',#6016);
#493=PLANE('',#6017);
#494=PLANE('',#6022);
#495=PLANE('',#6023);
#496=PLANE('',#6036);
#497=PLANE('',#6037);
#498=PLANE('',#6038);
#499=PLANE('',#6039);
#500=PLANE('',#6048);
#501=PLANE('',#6049);
#502=PLANE('',#6051);
#503=PLANE('',#6052);
#504=PLANE('',#6053);
#505=PLANE('',#6054);
#506=PLANE('',#6055);
#507=PLANE('',#6056);
#508=PLANE('',#6058);
#509=PLANE('',#6059);
#510=PLANE('',#6060);
#511=PLANE('',#6061);
#512=PLANE('',#6062);
#513=PLANE('',#6063);
#514=PLANE('',#6068);
#515=PLANE('',#6072);
#516=PLANE('',#6078);
#517=PLANE('',#6084);
#518=PLANE('',#6090);
#519=PLANE('',#6107);
#520=PLANE('',#6112);
#521=PLANE('',#6117);
#522=PLANE('',#6121);
#523=PLANE('',#6127);
#524=PLANE('',#6133);
#525=PLANE('',#6139);
#526=PLANE('',#6156);
#527=PLANE('',#6161);
#528=PLANE('',#6163);
#529=PLANE('',#6171);
#530=PLANE('',#6179);
#531=PLANE('',#6180);
#532=PLANE('',#6181);
#533=PLANE('',#6182);
#534=PLANE('',#6183);
#535=PLANE('',#6184);
#536=PLANE('',#6185);
#537=PLANE('',#6186);
#538=PLANE('',#6187);
#539=PLANE('',#6203);
#540=PLANE('',#6206);
#541=PLANE('',#6218);
#542=PLANE('',#6227);
#543=PLANE('',#6260);
#544=PLANE('',#6265);
#545=PLANE('',#6270);
#546=PLANE('',#6275);
#547=PLANE('',#6280);
#548=PLANE('',#6285);
#549=PLANE('',#6294);
#550=PLANE('',#6298);
#551=PLANE('',#6299);
#552=PLANE('',#6301);
#553=PLANE('',#6306);
#554=PLANE('',#6309);
#555=PLANE('',#6314);
#556=PLANE('',#6327);
#557=PLANE('',#6334);
#558=PLANE('',#6338);
#559=PLANE('',#6339);
#560=PLANE('',#6340);
#561=PLANE('',#6341);
#562=PLANE('',#6342);
#563=PLANE('',#6343);
#564=PLANE('',#6349);
#565=PLANE('',#6357);
#566=PLANE('',#6358);
#567=PLANE('',#6366);
#568=PLANE('',#6367);
#569=PLANE('',#6369);
#570=PLANE('',#6374);
#571=PLANE('',#6375);
#572=PLANE('',#6379);
#573=PLANE('',#6386);
#574=PLANE('',#6387);
#575=PLANE('',#6389);
#576=PLANE('',#6392);
#577=PLANE('',#6400);
#578=PLANE('',#6401);
#579=PLANE('',#6409);
#580=PLANE('',#6411);
#581=PLANE('',#6412);
#582=PLANE('',#6415);
#583=PLANE('',#6423);
#584=PLANE('',#6424);
#585=PLANE('',#6432);
#586=PLANE('',#6433);
#587=PLANE('',#6441);
#588=PLANE('',#6442);
#589=PLANE('',#6444);
#590=PLANE('',#6445);
#591=PLANE('',#6446);
#592=PLANE('',#6447);
#593=PLANE('',#6448);
#594=PLANE('',#6449);
#595=PLANE('',#6450);
#596=PLANE('',#6451);
#597=PLANE('',#6452);
#598=PLANE('',#6454);
#599=PLANE('',#6462);
#600=PLANE('',#6521);
#601=PLANE('',#6535);
#602=PLANE('',#6536);
#603=PLANE('',#6537);
#604=PLANE('',#6538);
#605=PLANE('',#6539);
#606=PLANE('',#6540);
#607=PLANE('',#6545);
#608=PLANE('',#6549);
#609=PLANE('',#6561);
#610=PLANE('',#6563);
#611=PLANE('',#6564);
#612=PLANE('',#6565);
#613=PLANE('',#6566);
#614=PLANE('',#6567);
#615=PLANE('',#6568);
#616=PLANE('',#6572);
#617=PLANE('',#6575);
#618=PLANE('',#6577);
#619=PLANE('',#6578);
#620=PLANE('',#6579);
#621=PLANE('',#6580);
#622=PLANE('',#6581);
#623=PLANE('',#6582);
#624=PLANE('',#6586);
#625=PLANE('',#6589);
#626=PLANE('',#6591);
#627=PLANE('',#6592);
#628=PLANE('',#6593);
#629=PLANE('',#6594);
#630=PLANE('',#6595);
#631=PLANE('',#6598);
#632=PLANE('',#6599);
#633=PLANE('',#6600);
#634=PLANE('',#6604);
#635=PLANE('',#6612);
#636=PLANE('',#6613);
#637=PLANE('',#6615);
#638=PLANE('',#6620);
#639=PLANE('',#6621);
#640=PLANE('',#6625);
#641=PLANE('',#6632);
#642=PLANE('',#6633);
#643=PLANE('',#6635);
#644=PLANE('',#6637);
#645=PLANE('',#6638);
#646=PLANE('',#6639);
#647=PLANE('',#6640);
#648=PLANE('',#6641);
#649=PLANE('',#6642);
#650=PLANE('',#6643);
#651=PLANE('',#6644);
#652=FACE_OUTER_BOUND('',#986,.T.);
#653=FACE_OUTER_BOUND('',#987,.T.);
#654=FACE_OUTER_BOUND('',#988,.T.);
#655=FACE_OUTER_BOUND('',#989,.T.);
#656=FACE_OUTER_BOUND('',#990,.T.);
#657=FACE_OUTER_BOUND('',#991,.T.);
#658=FACE_OUTER_BOUND('',#992,.T.);
#659=FACE_OUTER_BOUND('',#993,.T.);
#660=FACE_OUTER_BOUND('',#994,.T.);
#661=FACE_OUTER_BOUND('',#995,.T.);
#662=FACE_OUTER_BOUND('',#997,.T.);
#663=FACE_OUTER_BOUND('',#999,.T.);
#664=FACE_OUTER_BOUND('',#1000,.T.);
#665=FACE_OUTER_BOUND('',#1001,.T.);
#666=FACE_OUTER_BOUND('',#1002,.T.);
#667=FACE_OUTER_BOUND('',#1003,.T.);
#668=FACE_OUTER_BOUND('',#1004,.T.);
#669=FACE_OUTER_BOUND('',#1005,.T.);
#670=FACE_OUTER_BOUND('',#1006,.T.);
#671=FACE_OUTER_BOUND('',#1007,.T.);
#672=FACE_OUTER_BOUND('',#1008,.T.);
#673=FACE_OUTER_BOUND('',#1010,.T.);
#674=FACE_OUTER_BOUND('',#1012,.T.);
#675=FACE_OUTER_BOUND('',#1013,.T.);
#676=FACE_OUTER_BOUND('',#1015,.T.);
#677=FACE_OUTER_BOUND('',#1016,.T.);
#678=FACE_OUTER_BOUND('',#1018,.T.);
#679=FACE_OUTER_BOUND('',#1019,.T.);
#680=FACE_OUTER_BOUND('',#1021,.T.);
#681=FACE_OUTER_BOUND('',#1022,.T.);
#682=FACE_OUTER_BOUND('',#1024,.T.);
#683=FACE_OUTER_BOUND('',#1025,.T.);
#684=FACE_OUTER_BOUND('',#1026,.T.);
#685=FACE_OUTER_BOUND('',#1027,.T.);
#686=FACE_OUTER_BOUND('',#1028,.T.);
#687=FACE_OUTER_BOUND('',#1030,.T.);
#688=FACE_OUTER_BOUND('',#1032,.T.);
#689=FACE_OUTER_BOUND('',#1034,.T.);
#690=FACE_OUTER_BOUND('',#1036,.T.);
#691=FACE_OUTER_BOUND('',#1037,.T.);
#692=FACE_OUTER_BOUND('',#1038,.T.);
#693=FACE_OUTER_BOUND('',#1039,.T.);
#694=FACE_OUTER_BOUND('',#1040,.T.);
#695=FACE_OUTER_BOUND('',#1041,.T.);
#696=FACE_OUTER_BOUND('',#1042,.T.);
#697=FACE_OUTER_BOUND('',#1043,.T.);
#698=FACE_OUTER_BOUND('',#1058,.T.);
#699=FACE_OUTER_BOUND('',#1061,.T.);
#700=FACE_OUTER_BOUND('',#1062,.T.);
#701=FACE_OUTER_BOUND('',#1063,.T.);
#702=FACE_OUTER_BOUND('',#1064,.T.);
#703=FACE_OUTER_BOUND('',#1065,.T.);
#704=FACE_OUTER_BOUND('',#1066,.T.);
#705=FACE_OUTER_BOUND('',#1067,.T.);
#706=FACE_OUTER_BOUND('',#1068,.T.);
#707=FACE_OUTER_BOUND('',#1069,.T.);
#708=FACE_OUTER_BOUND('',#1070,.T.);
#709=FACE_OUTER_BOUND('',#1071,.T.);
#710=FACE_OUTER_BOUND('',#1072,.T.);
#711=FACE_OUTER_BOUND('',#1073,.T.);
#712=FACE_OUTER_BOUND('',#1079,.T.);
#713=FACE_OUTER_BOUND('',#1088,.T.);
#714=FACE_OUTER_BOUND('',#1089,.T.);
#715=FACE_OUTER_BOUND('',#1090,.T.);
#716=FACE_OUTER_BOUND('',#1091,.T.);
#717=FACE_OUTER_BOUND('',#1092,.T.);
#718=FACE_OUTER_BOUND('',#1093,.T.);
#719=FACE_OUTER_BOUND('',#1094,.T.);
#720=FACE_OUTER_BOUND('',#1095,.T.);
#721=FACE_OUTER_BOUND('',#1096,.T.);
#722=FACE_OUTER_BOUND('',#1097,.T.);
#723=FACE_OUTER_BOUND('',#1098,.T.);
#724=FACE_OUTER_BOUND('',#1099,.T.);
#725=FACE_OUTER_BOUND('',#1100,.T.);
#726=FACE_OUTER_BOUND('',#1101,.T.);
#727=FACE_OUTER_BOUND('',#1103,.T.);
#728=FACE_OUTER_BOUND('',#1105,.T.);
#729=FACE_OUTER_BOUND('',#1106,.T.);
#730=FACE_OUTER_BOUND('',#1108,.T.);
#731=FACE_OUTER_BOUND('',#1109,.T.);
#732=FACE_OUTER_BOUND('',#1111,.T.);
#733=FACE_OUTER_BOUND('',#1112,.T.);
#734=FACE_OUTER_BOUND('',#1114,.T.);
#735=FACE_OUTER_BOUND('',#1115,.T.);
#736=FACE_OUTER_BOUND('',#1116,.T.);
#737=FACE_OUTER_BOUND('',#1117,.T.);
#738=FACE_OUTER_BOUND('',#1118,.T.);
#739=FACE_OUTER_BOUND('',#1119,.T.);
#740=FACE_OUTER_BOUND('',#1121,.T.);
#741=FACE_OUTER_BOUND('',#1122,.T.);
#742=FACE_OUTER_BOUND('',#1123,.T.);
#743=FACE_OUTER_BOUND('',#1129,.T.);
#744=FACE_OUTER_BOUND('',#1130,.T.);
#745=FACE_OUTER_BOUND('',#1132,.T.);
#746=FACE_OUTER_BOUND('',#1134,.T.);
#747=FACE_OUTER_BOUND('',#1135,.T.);
#748=FACE_OUTER_BOUND('',#1137,.T.);
#749=FACE_OUTER_BOUND('',#1138,.T.);
#750=FACE_OUTER_BOUND('',#1140,.T.);
#751=FACE_OUTER_BOUND('',#1141,.T.);
#752=FACE_OUTER_BOUND('',#1143,.T.);
#753=FACE_OUTER_BOUND('',#1144,.T.);
#754=FACE_OUTER_BOUND('',#1145,.T.);
#755=FACE_OUTER_BOUND('',#1146,.T.);
#756=FACE_OUTER_BOUND('',#1147,.T.);
#757=FACE_OUTER_BOUND('',#1148,.T.);
#758=FACE_OUTER_BOUND('',#1150,.T.);
#759=FACE_OUTER_BOUND('',#1151,.T.);
#760=FACE_OUTER_BOUND('',#1152,.T.);
#761=FACE_OUTER_BOUND('',#1158,.T.);
#762=FACE_OUTER_BOUND('',#1159,.T.);
#763=FACE_OUTER_BOUND('',#1160,.T.);
#764=FACE_OUTER_BOUND('',#1161,.T.);
#765=FACE_OUTER_BOUND('',#1162,.T.);
#766=FACE_OUTER_BOUND('',#1164,.T.);
#767=FACE_OUTER_BOUND('',#1165,.T.);
#768=FACE_OUTER_BOUND('',#1166,.T.);
#769=FACE_OUTER_BOUND('',#1167,.T.);
#770=FACE_OUTER_BOUND('',#1168,.T.);
#771=FACE_OUTER_BOUND('',#1169,.T.);
#772=FACE_OUTER_BOUND('',#1170,.T.);
#773=FACE_OUTER_BOUND('',#1171,.T.);
#774=FACE_OUTER_BOUND('',#1172,.T.);
#775=FACE_OUTER_BOUND('',#1173,.T.);
#776=FACE_OUTER_BOUND('',#1174,.T.);
#777=FACE_OUTER_BOUND('',#1175,.T.);
#778=FACE_OUTER_BOUND('',#1176,.T.);
#779=FACE_OUTER_BOUND('',#1177,.T.);
#780=FACE_OUTER_BOUND('',#1178,.T.);
#781=FACE_OUTER_BOUND('',#1179,.T.);
#782=FACE_OUTER_BOUND('',#1180,.T.);
#783=FACE_OUTER_BOUND('',#1182,.T.);
#784=FACE_OUTER_BOUND('',#1183,.T.);
#785=FACE_OUTER_BOUND('',#1185,.T.);
#786=FACE_OUTER_BOUND('',#1186,.T.);
#787=FACE_OUTER_BOUND('',#1187,.T.);
#788=FACE_OUTER_BOUND('',#1188,.T.);
#789=FACE_OUTER_BOUND('',#1190,.T.);
#790=FACE_OUTER_BOUND('',#1191,.T.);
#791=FACE_OUTER_BOUND('',#1192,.T.);
#792=FACE_OUTER_BOUND('',#1193,.T.);
#793=FACE_OUTER_BOUND('',#1195,.T.);
#794=FACE_OUTER_BOUND('',#1196,.T.);
#795=FACE_OUTER_BOUND('',#1197,.T.);
#796=FACE_OUTER_BOUND('',#1198,.T.);
#797=FACE_OUTER_BOUND('',#1199,.T.);
#798=FACE_OUTER_BOUND('',#1200,.T.);
#799=FACE_OUTER_BOUND('',#1201,.T.);
#800=FACE_OUTER_BOUND('',#1202,.T.);
#801=FACE_OUTER_BOUND('',#1203,.T.);
#802=FACE_OUTER_BOUND('',#1204,.T.);
#803=FACE_OUTER_BOUND('',#1205,.T.);
#804=FACE_OUTER_BOUND('',#1206,.T.);
#805=FACE_OUTER_BOUND('',#1207,.T.);
#806=FACE_OUTER_BOUND('',#1208,.T.);
#807=FACE_OUTER_BOUND('',#1209,.T.);
#808=FACE_OUTER_BOUND('',#1210,.T.);
#809=FACE_OUTER_BOUND('',#1211,.T.);
#810=FACE_OUTER_BOUND('',#1212,.T.);
#811=FACE_OUTER_BOUND('',#1213,.T.);
#812=FACE_OUTER_BOUND('',#1214,.T.);
#813=FACE_OUTER_BOUND('',#1215,.T.);
#814=FACE_OUTER_BOUND('',#1216,.T.);
#815=FACE_OUTER_BOUND('',#1217,.T.);
#816=FACE_OUTER_BOUND('',#1218,.T.);
#817=FACE_OUTER_BOUND('',#1219,.T.);
#818=FACE_OUTER_BOUND('',#1220,.T.);
#819=FACE_OUTER_BOUND('',#1221,.T.);
#820=FACE_OUTER_BOUND('',#1223,.T.);
#821=FACE_OUTER_BOUND('',#1224,.T.);
#822=FACE_OUTER_BOUND('',#1226,.T.);
#823=FACE_OUTER_BOUND('',#1227,.T.);
#824=FACE_OUTER_BOUND('',#1229,.T.);
#825=FACE_OUTER_BOUND('',#1230,.T.);
#826=FACE_OUTER_BOUND('',#1232,.T.);
#827=FACE_OUTER_BOUND('',#1233,.T.);
#828=FACE_OUTER_BOUND('',#1235,.T.);
#829=FACE_OUTER_BOUND('',#1236,.T.);
#830=FACE_OUTER_BOUND('',#1237,.T.);
#831=FACE_OUTER_BOUND('',#1238,.T.);
#832=FACE_OUTER_BOUND('',#1239,.T.);
#833=FACE_OUTER_BOUND('',#1240,.T.);
#834=FACE_OUTER_BOUND('',#1243,.T.);
#835=FACE_OUTER_BOUND('',#1244,.T.);
#836=FACE_OUTER_BOUND('',#1245,.T.);
#837=FACE_OUTER_BOUND('',#1246,.T.);
#838=FACE_OUTER_BOUND('',#1247,.T.);
#839=FACE_OUTER_BOUND('',#1248,.T.);
#840=FACE_OUTER_BOUND('',#1251,.T.);
#841=FACE_OUTER_BOUND('',#1252,.T.);
#842=FACE_OUTER_BOUND('',#1253,.T.);
#843=FACE_OUTER_BOUND('',#1255,.T.);
#844=FACE_OUTER_BOUND('',#1256,.T.);
#845=FACE_OUTER_BOUND('',#1257,.T.);
#846=FACE_OUTER_BOUND('',#1258,.T.);
#847=FACE_OUTER_BOUND('',#1260,.T.);
#848=FACE_OUTER_BOUND('',#1261,.T.);
#849=FACE_OUTER_BOUND('',#1262,.T.);
#850=FACE_OUTER_BOUND('',#1263,.T.);
#851=FACE_OUTER_BOUND('',#1265,.T.);
#852=FACE_OUTER_BOUND('',#1267,.T.);
#853=FACE_OUTER_BOUND('',#1268,.T.);
#854=FACE_OUTER_BOUND('',#1269,.T.);
#855=FACE_OUTER_BOUND('',#1270,.T.);
#856=FACE_OUTER_BOUND('',#1271,.T.);
#857=FACE_OUTER_BOUND('',#1272,.T.);
#858=FACE_OUTER_BOUND('',#1273,.T.);
#859=FACE_OUTER_BOUND('',#1275,.T.);
#860=FACE_OUTER_BOUND('',#1277,.T.);
#861=FACE_OUTER_BOUND('',#1279,.T.);
#862=FACE_OUTER_BOUND('',#1281,.T.);
#863=FACE_OUTER_BOUND('',#1283,.T.);
#864=FACE_OUTER_BOUND('',#1285,.T.);
#865=FACE_OUTER_BOUND('',#1286,.T.);
#866=FACE_OUTER_BOUND('',#1287,.T.);
#867=FACE_OUTER_BOUND('',#1288,.T.);
#868=FACE_OUTER_BOUND('',#1289,.T.);
#869=FACE_OUTER_BOUND('',#1290,.T.);
#870=FACE_OUTER_BOUND('',#1291,.T.);
#871=FACE_OUTER_BOUND('',#1292,.T.);
#872=FACE_OUTER_BOUND('',#1294,.T.);
#873=FACE_OUTER_BOUND('',#1295,.T.);
#874=FACE_OUTER_BOUND('',#1296,.T.);
#875=FACE_OUTER_BOUND('',#1297,.T.);
#876=FACE_OUTER_BOUND('',#1299,.T.);
#877=FACE_OUTER_BOUND('',#1300,.T.);
#878=FACE_OUTER_BOUND('',#1301,.T.);
#879=FACE_OUTER_BOUND('',#1303,.T.);
#880=FACE_OUTER_BOUND('',#1305,.T.);
#881=FACE_OUTER_BOUND('',#1306,.T.);
#882=FACE_OUTER_BOUND('',#1307,.T.);
#883=FACE_OUTER_BOUND('',#1309,.T.);
#884=FACE_OUTER_BOUND('',#1311,.T.);
#885=FACE_OUTER_BOUND('',#1312,.T.);
#886=FACE_OUTER_BOUND('',#1313,.T.);
#887=FACE_OUTER_BOUND('',#1315,.T.);
#888=FACE_OUTER_BOUND('',#1317,.T.);
#889=FACE_OUTER_BOUND('',#1318,.T.);
#890=FACE_OUTER_BOUND('',#1319,.T.);
#891=FACE_OUTER_BOUND('',#1320,.T.);
#892=FACE_OUTER_BOUND('',#1321,.T.);
#893=FACE_OUTER_BOUND('',#1322,.T.);
#894=FACE_OUTER_BOUND('',#1323,.T.);
#895=FACE_OUTER_BOUND('',#1324,.T.);
#896=FACE_OUTER_BOUND('',#1325,.T.);
#897=FACE_OUTER_BOUND('',#1326,.T.);
#898=FACE_OUTER_BOUND('',#1327,.T.);
#899=FACE_OUTER_BOUND('',#1328,.T.);
#900=FACE_OUTER_BOUND('',#1329,.T.);
#901=FACE_OUTER_BOUND('',#1330,.T.);
#902=FACE_OUTER_BOUND('',#1332,.T.);
#903=FACE_OUTER_BOUND('',#1333,.T.);
#904=FACE_OUTER_BOUND('',#1334,.T.);
#905=FACE_OUTER_BOUND('',#1335,.T.);
#906=FACE_OUTER_BOUND('',#1336,.T.);
#907=FACE_OUTER_BOUND('',#1337,.T.);
#908=FACE_OUTER_BOUND('',#1338,.T.);
#909=FACE_OUTER_BOUND('',#1339,.T.);
#910=FACE_OUTER_BOUND('',#1340,.T.);
#911=FACE_OUTER_BOUND('',#1341,.T.);
#912=FACE_OUTER_BOUND('',#1342,.T.);
#913=FACE_OUTER_BOUND('',#1343,.T.);
#914=FACE_OUTER_BOUND('',#1344,.T.);
#915=FACE_OUTER_BOUND('',#1345,.T.);
#916=FACE_OUTER_BOUND('',#1350,.T.);
#917=FACE_OUTER_BOUND('',#1351,.T.);
#918=FACE_OUTER_BOUND('',#1352,.T.);
#919=FACE_OUTER_BOUND('',#1353,.T.);
#920=FACE_OUTER_BOUND('',#1354,.T.);
#921=FACE_OUTER_BOUND('',#1355,.T.);
#922=FACE_OUTER_BOUND('',#1356,.T.);
#923=FACE_OUTER_BOUND('',#1357,.T.);
#924=FACE_OUTER_BOUND('',#1359,.T.);
#925=FACE_OUTER_BOUND('',#1361,.T.);
#926=FACE_OUTER_BOUND('',#1362,.T.);
#927=FACE_OUTER_BOUND('',#1363,.T.);
#928=FACE_OUTER_BOUND('',#1364,.T.);
#929=FACE_OUTER_BOUND('',#1365,.T.);
#930=FACE_OUTER_BOUND('',#1366,.T.);
#931=FACE_OUTER_BOUND('',#1367,.T.);
#932=FACE_OUTER_BOUND('',#1368,.T.);
#933=FACE_OUTER_BOUND('',#1369,.T.);
#934=FACE_OUTER_BOUND('',#1370,.T.);
#935=FACE_OUTER_BOUND('',#1371,.T.);
#936=FACE_OUTER_BOUND('',#1373,.T.);
#937=FACE_OUTER_BOUND('',#1374,.T.);
#938=FACE_OUTER_BOUND('',#1375,.T.);
#939=FACE_OUTER_BOUND('',#1376,.T.);
#940=FACE_OUTER_BOUND('',#1377,.T.);
#941=FACE_OUTER_BOUND('',#1378,.T.);
#942=FACE_OUTER_BOUND('',#1379,.T.);
#943=FACE_OUTER_BOUND('',#1380,.T.);
#944=FACE_OUTER_BOUND('',#1381,.T.);
#945=FACE_OUTER_BOUND('',#1382,.T.);
#946=FACE_OUTER_BOUND('',#1384,.T.);
#947=FACE_OUTER_BOUND('',#1385,.T.);
#948=FACE_OUTER_BOUND('',#1386,.T.);
#949=FACE_OUTER_BOUND('',#1387,.T.);
#950=FACE_OUTER_BOUND('',#1388,.T.);
#951=FACE_OUTER_BOUND('',#1389,.T.);
#952=FACE_OUTER_BOUND('',#1390,.T.);
#953=FACE_OUTER_BOUND('',#1391,.T.);
#954=FACE_OUTER_BOUND('',#1392,.T.);
#955=FACE_OUTER_BOUND('',#1393,.T.);
#956=FACE_OUTER_BOUND('',#1394,.T.);
#957=FACE_OUTER_BOUND('',#1395,.T.);
#958=FACE_OUTER_BOUND('',#1396,.T.);
#959=FACE_OUTER_BOUND('',#1398,.T.);
#960=FACE_OUTER_BOUND('',#1399,.T.);
#961=FACE_OUTER_BOUND('',#1400,.T.);
#962=FACE_OUTER_BOUND('',#1401,.T.);
#963=FACE_OUTER_BOUND('',#1402,.T.);
#964=FACE_OUTER_BOUND('',#1404,.T.);
#965=FACE_OUTER_BOUND('',#1406,.T.);
#966=FACE_OUTER_BOUND('',#1407,.T.);
#967=FACE_OUTER_BOUND('',#1408,.T.);
#968=FACE_OUTER_BOUND('',#1409,.T.);
#969=FACE_OUTER_BOUND('',#1410,.T.);
#970=FACE_OUTER_BOUND('',#1411,.T.);
#971=FACE_OUTER_BOUND('',#1412,.T.);
#972=FACE_OUTER_BOUND('',#1414,.T.);
#973=FACE_OUTER_BOUND('',#1416,.T.);
#974=FACE_OUTER_BOUND('',#1418,.T.);
#975=FACE_OUTER_BOUND('',#1420,.T.);
#976=FACE_OUTER_BOUND('',#1421,.T.);
#977=FACE_OUTER_BOUND('',#1422,.T.);
#978=FACE_OUTER_BOUND('',#1423,.T.);
#979=FACE_OUTER_BOUND('',#1424,.T.);
#980=FACE_OUTER_BOUND('',#1425,.T.);
#981=FACE_OUTER_BOUND('',#1426,.T.);
#982=FACE_OUTER_BOUND('',#1427,.T.);
#983=FACE_OUTER_BOUND('',#1428,.T.);
#984=FACE_OUTER_BOUND('',#1430,.T.);
#985=FACE_OUTER_BOUND('',#1431,.T.);
#986=EDGE_LOOP('',(#3708,#3709,#3710,#3711));
#987=EDGE_LOOP('',(#3712));
#988=EDGE_LOOP('',(#3713,#3714,#3715,#3716));
#989=EDGE_LOOP('',(#3717));
#990=EDGE_LOOP('',(#3718,#3719,#3720,#3721));
#991=EDGE_LOOP('',(#3722));
#992=EDGE_LOOP('',(#3723,#3724,#3725,#3726));
#993=EDGE_LOOP('',(#3727));
#994=EDGE_LOOP('',(#3728,#3729,#3730,#3731));
#995=EDGE_LOOP('',(#3732));
#996=EDGE_LOOP('',(#3733));
#997=EDGE_LOOP('',(#3734,#3735,#3736,#3737));
#998=EDGE_LOOP('',(#3738));
#999=EDGE_LOOP('',(#3739,#3740,#3741,#3742));
#1000=EDGE_LOOP('',(#3743));
#1001=EDGE_LOOP('',(#3744,#3745,#3746,#3747));
#1002=EDGE_LOOP('',(#3748));
#1003=EDGE_LOOP('',(#3749,#3750,#3751,#3752));
#1004=EDGE_LOOP('',(#3753));
#1005=EDGE_LOOP('',(#3754,#3755,#3756,#3757));
#1006=EDGE_LOOP('',(#3758));
#1007=EDGE_LOOP('',(#3759,#3760,#3761,#3762));
#1008=EDGE_LOOP('',(#3763));
#1009=EDGE_LOOP('',(#3764));
#1010=EDGE_LOOP('',(#3765,#3766,#3767,#3768));
#1011=EDGE_LOOP('',(#3769));
#1012=EDGE_LOOP('',(#3770,#3771,#3772,#3773));
#1013=EDGE_LOOP('',(#3774));
#1014=EDGE_LOOP('',(#3775));
#1015=EDGE_LOOP('',(#3776,#3777,#3778,#3779));
#1016=EDGE_LOOP('',(#3780));
#1017=EDGE_LOOP('',(#3781));
#1018=EDGE_LOOP('',(#3782,#3783,#3784,#3785));
#1019=EDGE_LOOP('',(#3786));
#1020=EDGE_LOOP('',(#3787));
#1021=EDGE_LOOP('',(#3788,#3789,#3790,#3791));
#1022=EDGE_LOOP('',(#3792));
#1023=EDGE_LOOP('',(#3793));
#1024=EDGE_LOOP('',(#3794,#3795,#3796,#3797));
#1025=EDGE_LOOP('',(#3798,#3799,#3800,#3801));
#1026=EDGE_LOOP('',(#3802,#3803,#3804,#3805));
#1027=EDGE_LOOP('',(#3806,#3807,#3808,#3809));
#1028=EDGE_LOOP('',(#3810));
#1029=EDGE_LOOP('',(#3811));
#1030=EDGE_LOOP('',(#3812));
#1031=EDGE_LOOP('',(#3813));
#1032=EDGE_LOOP('',(#3814));
#1033=EDGE_LOOP('',(#3815));
#1034=EDGE_LOOP('',(#3816));
#1035=EDGE_LOOP('',(#3817));
#1036=EDGE_LOOP('',(#3818));
#1037=EDGE_LOOP('',(#3819));
#1038=EDGE_LOOP('',(#3820,#3821,#3822,#3823));
#1039=EDGE_LOOP('',(#3824,#3825,#3826,#3827));
#1040=EDGE_LOOP('',(#3828,#3829,#3830,#3831));
#1041=EDGE_LOOP('',(#3832,#3833,#3834,#3835));
#1042=EDGE_LOOP('',(#3836,#3837,#3838,#3839));
#1043=EDGE_LOOP('',(#3840,#3841,#3842,#3843));
#1044=EDGE_LOOP('',(#3844));
#1045=EDGE_LOOP('',(#3845));
#1046=EDGE_LOOP('',(#3846));
#1047=EDGE_LOOP('',(#3847));
#1048=EDGE_LOOP('',(#3848));
#1049=EDGE_LOOP('',(#3849));
#1050=EDGE_LOOP('',(#3850));
#1051=EDGE_LOOP('',(#3851));
#1052=EDGE_LOOP('',(#3852));
#1053=EDGE_LOOP('',(#3853));
#1054=EDGE_LOOP('',(#3854));
#1055=EDGE_LOOP('',(#3855));
#1056=EDGE_LOOP('',(#3856));
#1057=EDGE_LOOP('',(#3857));
#1058=EDGE_LOOP('',(#3858,#3859,#3860,#3861));
#1059=EDGE_LOOP('',(#3862));
#1060=EDGE_LOOP('',(#3863));
#1061=EDGE_LOOP('',(#3864,#3865,#3866,#3867));
#1062=EDGE_LOOP('',(#3868,#3869,#3870,#3871));
#1063=EDGE_LOOP('',(#3872,#3873,#3874,#3875));
#1064=EDGE_LOOP('',(#3876,#3877,#3878,#3879));
#1065=EDGE_LOOP('',(#3880,#3881,#3882,#3883));
#1066=EDGE_LOOP('',(#3884,#3885,#3886,#3887));
#1067=EDGE_LOOP('',(#3888,#3889,#3890,#3891));
#1068=EDGE_LOOP('',(#3892,#3893,#3894,#3895));
#1069=EDGE_LOOP('',(#3896,#3897,#3898,#3899));
#1070=EDGE_LOOP('',(#3900,#3901,#3902,#3903));
#1071=EDGE_LOOP('',(#3904,#3905,#3906,#3907));
#1072=EDGE_LOOP('',(#3908,#3909,#3910,#3911));
#1073=EDGE_LOOP('',(#3912,#3913,#3914,#3915));
#1074=EDGE_LOOP('',(#3916,#3917,#3918,#3919));
#1075=EDGE_LOOP('',(#3920));
#1076=EDGE_LOOP('',(#3921));
#1077=EDGE_LOOP('',(#3922));
#1078=EDGE_LOOP('',(#3923));
#1079=EDGE_LOOP('',(#3924,#3925,#3926,#3927));
#1080=EDGE_LOOP('',(#3928));
#1081=EDGE_LOOP('',(#3929));
#1082=EDGE_LOOP('',(#3930));
#1083=EDGE_LOOP('',(#3931));
#1084=EDGE_LOOP('',(#3932));
#1085=EDGE_LOOP('',(#3933));
#1086=EDGE_LOOP('',(#3934));
#1087=EDGE_LOOP('',(#3935));
#1088=EDGE_LOOP('',(#3936,#3937,#3938,#3939));
#1089=EDGE_LOOP('',(#3940,#3941,#3942,#3943));
#1090=EDGE_LOOP('',(#3944,#3945,#3946,#3947));
#1091=EDGE_LOOP('',(#3948,#3949,#3950,#3951));
#1092=EDGE_LOOP('',(#3952,#3953,#3954,#3955));
#1093=EDGE_LOOP('',(#3956,#3957,#3958,#3959));
#1094=EDGE_LOOP('',(#3960,#3961,#3962,#3963));
#1095=EDGE_LOOP('',(#3964,#3965,#3966,#3967));
#1096=EDGE_LOOP('',(#3968,#3969,#3970,#3971));
#1097=EDGE_LOOP('',(#3972,#3973,#3974,#3975));
#1098=EDGE_LOOP('',(#3976,#3977,#3978,#3979));
#1099=EDGE_LOOP('',(#3980,#3981,#3982,#3983));
#1100=EDGE_LOOP('',(#3984,#3985,#3986,#3987));
#1101=EDGE_LOOP('',(#3988,#3989,#3990));
#1102=EDGE_LOOP('',(#3991));
#1103=EDGE_LOOP('',(#3992,#3993));
#1104=EDGE_LOOP('',(#3994));
#1105=EDGE_LOOP('',(#3995,#3996,#3997,#3998));
#1106=EDGE_LOOP('',(#3999,#4000));
#1107=EDGE_LOOP('',(#4001));
#1108=EDGE_LOOP('',(#4002,#4003,#4004,#4005));
#1109=EDGE_LOOP('',(#4006,#4007));
#1110=EDGE_LOOP('',(#4008));
#1111=EDGE_LOOP('',(#4009,#4010,#4011,#4012));
#1112=EDGE_LOOP('',(#4013,#4014,#4015,#4016,#4017,#4018,#4019,#4020));
#1113=EDGE_LOOP('',(#4021));
#1114=EDGE_LOOP('',(#4022,#4023,#4024,#4025));
#1115=EDGE_LOOP('',(#4026,#4027,#4028,#4029));
#1116=EDGE_LOOP('',(#4030,#4031,#4032,#4033));
#1117=EDGE_LOOP('',(#4034,#4035,#4036,#4037));
#1118=EDGE_LOOP('',(#4038,#4039,#4040,#4041));
#1119=EDGE_LOOP('',(#4042));
#1120=EDGE_LOOP('',(#4043));
#1121=EDGE_LOOP('',(#4044,#4045,#4046,#4047));
#1122=EDGE_LOOP('',(#4048,#4049,#4050,#4051,#4052,#4053,#4054,#4055,#4056,
#4057,#4058,#4059,#4060,#4061,#4062,#4063,#4064,#4065,#4066,#4067));
#1123=EDGE_LOOP('',(#4068));
#1124=EDGE_LOOP('',(#4069));
#1125=EDGE_LOOP('',(#4070));
#1126=EDGE_LOOP('',(#4071));
#1127=EDGE_LOOP('',(#4072));
#1128=EDGE_LOOP('',(#4073));
#1129=EDGE_LOOP('',(#4074,#4075,#4076,#4077));
#1130=EDGE_LOOP('',(#4078,#4079,#4080));
#1131=EDGE_LOOP('',(#4081));
#1132=EDGE_LOOP('',(#4082,#4083));
#1133=EDGE_LOOP('',(#4084));
#1134=EDGE_LOOP('',(#4085,#4086,#4087,#4088));
#1135=EDGE_LOOP('',(#4089,#4090));
#1136=EDGE_LOOP('',(#4091));
#1137=EDGE_LOOP('',(#4092,#4093,#4094,#4095));
#1138=EDGE_LOOP('',(#4096,#4097));
#1139=EDGE_LOOP('',(#4098));
#1140=EDGE_LOOP('',(#4099,#4100,#4101,#4102));
#1141=EDGE_LOOP('',(#4103,#4104,#4105,#4106,#4107,#4108,#4109,#4110));
#1142=EDGE_LOOP('',(#4111));
#1143=EDGE_LOOP('',(#4112,#4113,#4114,#4115));
#1144=EDGE_LOOP('',(#4116,#4117,#4118,#4119));
#1145=EDGE_LOOP('',(#4120,#4121,#4122,#4123));
#1146=EDGE_LOOP('',(#4124,#4125,#4126,#4127));
#1147=EDGE_LOOP('',(#4128,#4129,#4130,#4131));
#1148=EDGE_LOOP('',(#4132));
#1149=EDGE_LOOP('',(#4133));
#1150=EDGE_LOOP('',(#4134,#4135,#4136,#4137));
#1151=EDGE_LOOP('',(#4138,#4139,#4140,#4141,#4142,#4143,#4144,#4145,#4146,
#4147,#4148,#4149,#4150,#4151,#4152,#4153,#4154,#4155,#4156,#4157));
#1152=EDGE_LOOP('',(#4158));
#1153=EDGE_LOOP('',(#4159));
#1154=EDGE_LOOP('',(#4160));
#1155=EDGE_LOOP('',(#4161));
#1156=EDGE_LOOP('',(#4162));
#1157=EDGE_LOOP('',(#4163));
#1158=EDGE_LOOP('',(#4164));
#1159=EDGE_LOOP('',(#4165,#4166,#4167,#4168));
#1160=EDGE_LOOP('',(#4169,#4170,#4171,#4172));
#1161=EDGE_LOOP('',(#4173,#4174,#4175,#4176));
#1162=EDGE_LOOP('',(#4177));
#1163=EDGE_LOOP('',(#4178));
#1164=EDGE_LOOP('',(#4179,#4180,#4181,#4182));
#1165=EDGE_LOOP('',(#4183,#4184,#4185,#4186));
#1166=EDGE_LOOP('',(#4187,#4188,#4189,#4190));
#1167=EDGE_LOOP('',(#4191));
#1168=EDGE_LOOP('',(#4192,#4193,#4194,#4195));
#1169=EDGE_LOOP('',(#4196,#4197,#4198,#4199));
#1170=EDGE_LOOP('',(#4200,#4201,#4202,#4203));
#1171=EDGE_LOOP('',(#4204,#4205,#4206,#4207));
#1172=EDGE_LOOP('',(#4208,#4209,#4210,#4211));
#1173=EDGE_LOOP('',(#4212,#4213,#4214,#4215));
#1174=EDGE_LOOP('',(#4216,#4217,#4218,#4219,#4220,#4221));
#1175=EDGE_LOOP('',(#4222,#4223,#4224,#4225,#4226,#4227));
#1176=EDGE_LOOP('',(#4228,#4229,#4230,#4231,#4232,#4233));
#1177=EDGE_LOOP('',(#4234,#4235,#4236,#4237,#4238));
#1178=EDGE_LOOP('',(#4239,#4240,#4241,#4242));
#1179=EDGE_LOOP('',(#4243,#4244,#4245,#4246));
#1180=EDGE_LOOP('',(#4247));
#1181=EDGE_LOOP('',(#4248));
#1182=EDGE_LOOP('',(#4249,#4250,#4251,#4252,#4253));
#1183=EDGE_LOOP('',(#4254));
#1184=EDGE_LOOP('',(#4255));
#1185=EDGE_LOOP('',(#4256,#4257,#4258,#4259));
#1186=EDGE_LOOP('',(#4260,#4261,#4262,#4263,#4264,#4265));
#1187=EDGE_LOOP('',(#4266,#4267,#4268,#4269,#4270));
#1188=EDGE_LOOP('',(#4271));
#1189=EDGE_LOOP('',(#4272));
#1190=EDGE_LOOP('',(#4273,#4274,#4275,#4276));
#1191=EDGE_LOOP('',(#4277,#4278,#4279,#4280));
#1192=EDGE_LOOP('',(#4281,#4282,#4283,#4284));
#1193=EDGE_LOOP('',(#4285));
#1194=EDGE_LOOP('',(#4286));
#1195=EDGE_LOOP('',(#4287,#4288,#4289,#4290,#4291));
#1196=EDGE_LOOP('',(#4292,#4293));
#1197=EDGE_LOOP('',(#4294,#4295));
#1198=EDGE_LOOP('',(#4296,#4297));
#1199=EDGE_LOOP('',(#4298,#4299));
#1200=EDGE_LOOP('',(#4300,#4301));
#1201=EDGE_LOOP('',(#4302,#4303));
#1202=EDGE_LOOP('',(#4304,#4305));
#1203=EDGE_LOOP('',(#4306,#4307));
#1204=EDGE_LOOP('',(#4308,#4309,#4310,#4311));
#1205=EDGE_LOOP('',(#4312,#4313,#4314,#4315,#4316,#4317,#4318,#4319,#4320,
#4321,#4322,#4323,#4324,#4325,#4326,#4327,#4328,#4329,#4330,#4331));
#1206=EDGE_LOOP('',(#4332,#4333,#4334,#4335));
#1207=EDGE_LOOP('',(#4336,#4337,#4338,#4339));
#1208=EDGE_LOOP('',(#4340,#4341,#4342,#4343));
#1209=EDGE_LOOP('',(#4344,#4345,#4346,#4347));
#1210=EDGE_LOOP('',(#4348,#4349,#4350,#4351));
#1211=EDGE_LOOP('',(#4352,#4353,#4354,#4355,#4356,#4357));
#1212=EDGE_LOOP('',(#4358,#4359,#4360,#4361));
#1213=EDGE_LOOP('',(#4362,#4363,#4364,#4365));
#1214=EDGE_LOOP('',(#4366,#4367,#4368,#4369));
#1215=EDGE_LOOP('',(#4370,#4371,#4372,#4373));
#1216=EDGE_LOOP('',(#4374,#4375,#4376,#4377));
#1217=EDGE_LOOP('',(#4378,#4379,#4380,#4381));
#1218=EDGE_LOOP('',(#4382,#4383,#4384,#4385,#4386,#4387,#4388,#4389,#4390,
#4391,#4392,#4393,#4394,#4395,#4396,#4397,#4398,#4399,#4400,#4401));
#1219=EDGE_LOOP('',(#4402,#4403,#4404,#4405));
#1220=EDGE_LOOP('',(#4406,#4407,#4408,#4409));
#1221=EDGE_LOOP('',(#4410));
#1222=EDGE_LOOP('',(#4411));
#1223=EDGE_LOOP('',(#4412,#4413,#4414,#4415));
#1224=EDGE_LOOP('',(#4416));
#1225=EDGE_LOOP('',(#4417));
#1226=EDGE_LOOP('',(#4418,#4419,#4420,#4421));
#1227=EDGE_LOOP('',(#4422));
#1228=EDGE_LOOP('',(#4423));
#1229=EDGE_LOOP('',(#4424,#4425,#4426,#4427));
#1230=EDGE_LOOP('',(#4428));
#1231=EDGE_LOOP('',(#4429));
#1232=EDGE_LOOP('',(#4430,#4431,#4432,#4433));
#1233=EDGE_LOOP('',(#4434));
#1234=EDGE_LOOP('',(#4435));
#1235=EDGE_LOOP('',(#4436,#4437,#4438,#4439));
#1236=EDGE_LOOP('',(#4440,#4441,#4442,#4443));
#1237=EDGE_LOOP('',(#4444));
#1238=EDGE_LOOP('',(#4445,#4446,#4447,#4448));
#1239=EDGE_LOOP('',(#4449,#4450,#4451,#4452));
#1240=EDGE_LOOP('',(#4453,#4454,#4455,#4456,#4457,#4458,#4459,#4460));
#1241=EDGE_LOOP('',(#4461));
#1242=EDGE_LOOP('',(#4462));
#1243=EDGE_LOOP('',(#4463,#4464,#4465,#4466));
#1244=EDGE_LOOP('',(#4467,#4468,#4469,#4470));
#1245=EDGE_LOOP('',(#4471,#4472,#4473,#4474));
#1246=EDGE_LOOP('',(#4475,#4476,#4477,#4478));
#1247=EDGE_LOOP('',(#4479,#4480,#4481,#4482));
#1248=EDGE_LOOP('',(#4483,#4484,#4485,#4486,#4487,#4488,#4489,#4490));
#1249=EDGE_LOOP('',(#4491));
#1250=EDGE_LOOP('',(#4492));
#1251=EDGE_LOOP('',(#4493,#4494,#4495,#4496));
#1252=EDGE_LOOP('',(#4497,#4498,#4499,#4500));
#1253=EDGE_LOOP('',(#4501));
#1254=EDGE_LOOP('',(#4502));
#1255=EDGE_LOOP('',(#4503,#4504,#4505,#4506));
#1256=EDGE_LOOP('',(#4507,#4508,#4509,#4510));
#1257=EDGE_LOOP('',(#4511,#4512,#4513,#4514));
#1258=EDGE_LOOP('',(#4515));
#1259=EDGE_LOOP('',(#4516));
#1260=EDGE_LOOP('',(#4517));
#1261=EDGE_LOOP('',(#4518,#4519,#4520,#4521));
#1262=EDGE_LOOP('',(#4522,#4523,#4524,#4525));
#1263=EDGE_LOOP('',(#4526));
#1264=EDGE_LOOP('',(#4527));
#1265=EDGE_LOOP('',(#4528));
#1266=EDGE_LOOP('',(#4529));
#1267=EDGE_LOOP('',(#4530,#4531,#4532));
#1268=EDGE_LOOP('',(#4533,#4534,#4535,#4536,#4537,#4538,#4539,#4540));
#1269=EDGE_LOOP('',(#4541,#4542));
#1270=EDGE_LOOP('',(#4543,#4544));
#1271=EDGE_LOOP('',(#4545,#4546,#4547,#4548,#4549,#4550,#4551,#4552,#4553,
#4554,#4555));
#1272=EDGE_LOOP('',(#4556,#4557));
#1273=EDGE_LOOP('',(#4558,#4559,#4560,#4561,#4562,#4563,#4564,#4565,#4566,
#4567,#4568,#4569));
#1274=EDGE_LOOP('',(#4570,#4571,#4572,#4573));
#1275=EDGE_LOOP('',(#4574,#4575,#4576,#4577,#4578,#4579,#4580,#4581,#4582));
#1276=EDGE_LOOP('',(#4583));
#1277=EDGE_LOOP('',(#4584));
#1278=EDGE_LOOP('',(#4585));
#1279=EDGE_LOOP('',(#4586));
#1280=EDGE_LOOP('',(#4587));
#1281=EDGE_LOOP('',(#4588));
#1282=EDGE_LOOP('',(#4589));
#1283=EDGE_LOOP('',(#4590));
#1284=EDGE_LOOP('',(#4591));
#1285=EDGE_LOOP('',(#4592,#4593,#4594,#4595));
#1286=EDGE_LOOP('',(#4596,#4597,#4598,#4599));
#1287=EDGE_LOOP('',(#4600,#4601,#4602,#4603));
#1288=EDGE_LOOP('',(#4604));
#1289=EDGE_LOOP('',(#4605));
#1290=EDGE_LOOP('',(#4606,#4607,#4608,#4609));
#1291=EDGE_LOOP('',(#4610,#4611,#4612,#4613));
#1292=EDGE_LOOP('',(#4614,#4615,#4616,#4617));
#1293=EDGE_LOOP('',(#4618));
#1294=EDGE_LOOP('',(#4619,#4620,#4621,#4622));
#1295=EDGE_LOOP('',(#4623,#4624,#4625,#4626));
#1296=EDGE_LOOP('',(#4627,#4628,#4629,#4630));
#1297=EDGE_LOOP('',(#4631,#4632,#4633,#4634));
#1298=EDGE_LOOP('',(#4635));
#1299=EDGE_LOOP('',(#4636,#4637,#4638,#4639));
#1300=EDGE_LOOP('',(#4640,#4641,#4642,#4643));
#1301=EDGE_LOOP('',(#4644));
#1302=EDGE_LOOP('',(#4645));
#1303=EDGE_LOOP('',(#4646));
#1304=EDGE_LOOP('',(#4647));
#1305=EDGE_LOOP('',(#4648,#4649,#4650,#4651));
#1306=EDGE_LOOP('',(#4652,#4653,#4654,#4655));
#1307=EDGE_LOOP('',(#4656));
#1308=EDGE_LOOP('',(#4657));
#1309=EDGE_LOOP('',(#4658));
#1310=EDGE_LOOP('',(#4659));
#1311=EDGE_LOOP('',(#4660,#4661,#4662,#4663));
#1312=EDGE_LOOP('',(#4664,#4665,#4666,#4667));
#1313=EDGE_LOOP('',(#4668));
#1314=EDGE_LOOP('',(#4669));
#1315=EDGE_LOOP('',(#4670));
#1316=EDGE_LOOP('',(#4671));
#1317=EDGE_LOOP('',(#4672,#4673,#4674,#4675));
#1318=EDGE_LOOP('',(#4676,#4677,#4678,#4679));
#1319=EDGE_LOOP('',(#4680,#4681,#4682,#4683));
#1320=EDGE_LOOP('',(#4684,#4685,#4686,#4687));
#1321=EDGE_LOOP('',(#4688,#4689,#4690,#4691));
#1322=EDGE_LOOP('',(#4692,#4693,#4694,#4695));
#1323=EDGE_LOOP('',(#4696,#4697,#4698,#4699,#4700,#4701));
#1324=EDGE_LOOP('',(#4702,#4703,#4704,#4705,#4706,#4707));
#1325=EDGE_LOOP('',(#4708));
#1326=EDGE_LOOP('',(#4709));
#1327=EDGE_LOOP('',(#4710,#4711,#4712,#4713));
#1328=EDGE_LOOP('',(#4714,#4715,#4716,#4717));
#1329=EDGE_LOOP('',(#4718,#4719,#4720,#4721));
#1330=EDGE_LOOP('',(#4722));
#1331=EDGE_LOOP('',(#4723));
#1332=EDGE_LOOP('',(#4724,#4725,#4726,#4727));
#1333=EDGE_LOOP('',(#4728,#4729,#4730,#4731));
#1334=EDGE_LOOP('',(#4732,#4733,#4734,#4735));
#1335=EDGE_LOOP('',(#4736,#4737,#4738,#4739));
#1336=EDGE_LOOP('',(#4740,#4741,#4742,#4743));
#1337=EDGE_LOOP('',(#4744,#4745,#4746,#4747));
#1338=EDGE_LOOP('',(#4748,#4749,#4750,#4751));
#1339=EDGE_LOOP('',(#4752,#4753,#4754,#4755));
#1340=EDGE_LOOP('',(#4756,#4757,#4758,#4759));
#1341=EDGE_LOOP('',(#4760,#4761,#4762,#4763));
#1342=EDGE_LOOP('',(#4764,#4765,#4766,#4767));
#1343=EDGE_LOOP('',(#4768,#4769,#4770,#4771));
#1344=EDGE_LOOP('',(#4772,#4773,#4774,#4775));
#1345=EDGE_LOOP('',(#4776,#4777,#4778,#4779,#4780,#4781,#4782,#4783,#4784,
#4785,#4786,#4787,#4788,#4789,#4790,#4791,#4792,#4793,#4794,#4795,#4796,
#4797,#4798,#4799,#4800,#4801,#4802,#4803,#4804,#4805,#4806,#4807,#4808,
#4809,#4810,#4811,#4812,#4813,#4814,#4815));
#1346=EDGE_LOOP('',(#4816));
#1347=EDGE_LOOP('',(#4817));
#1348=EDGE_LOOP('',(#4818));
#1349=EDGE_LOOP('',(#4819));
#1350=EDGE_LOOP('',(#4820,#4821,#4822,#4823));
#1351=EDGE_LOOP('',(#4824,#4825,#4826,#4827));
#1352=EDGE_LOOP('',(#4828,#4829,#4830,#4831));
#1353=EDGE_LOOP('',(#4832,#4833,#4834,#4835));
#1354=EDGE_LOOP('',(#4836,#4837,#4838,#4839));
#1355=EDGE_LOOP('',(#4840,#4841,#4842,#4843));
#1356=EDGE_LOOP('',(#4844,#4845,#4846,#4847));
#1357=EDGE_LOOP('',(#4848,#4849,#4850,#4851,#4852,#4853,#4854,#4855,#4856,
#4857,#4858,#4859));
#1358=EDGE_LOOP('',(#4860));
#1359=EDGE_LOOP('',(#4861,#4862,#4863,#4864,#4865,#4866,#4867,#4868,#4869,
#4870,#4871,#4872));
#1360=EDGE_LOOP('',(#4873));
#1361=EDGE_LOOP('',(#4874,#4875));
#1362=EDGE_LOOP('',(#4876,#4877,#4878,#4879,#4880,#4881,#4882,#4883));
#1363=EDGE_LOOP('',(#4884,#4885,#4886,#4887,#4888,#4889,#4890,#4891,#4892,
#4893,#4894,#4895,#4896,#4897,#4898,#4899,#4900,#4901,#4902,#4903));
#1364=EDGE_LOOP('',(#4904,#4905,#4906,#4907));
#1365=EDGE_LOOP('',(#4908,#4909,#4910,#4911));
#1366=EDGE_LOOP('',(#4912,#4913,#4914,#4915));
#1367=EDGE_LOOP('',(#4916,#4917,#4918,#4919));
#1368=EDGE_LOOP('',(#4920,#4921,#4922,#4923));
#1369=EDGE_LOOP('',(#4924,#4925,#4926,#4927));
#1370=EDGE_LOOP('',(#4928,#4929,#4930,#4931));
#1371=EDGE_LOOP('',(#4932,#4933,#4934,#4935,#4936,#4937,#4938,#4939,#4940,
#4941,#4942,#4943));
#1372=EDGE_LOOP('',(#4944));
#1373=EDGE_LOOP('',(#4945,#4946,#4947));
#1374=EDGE_LOOP('',(#4948,#4949,#4950,#4951,#4952,#4953,#4954,#4955));
#1375=EDGE_LOOP('',(#4956,#4957,#4958,#4959));
#1376=EDGE_LOOP('',(#4960,#4961,#4962,#4963));
#1377=EDGE_LOOP('',(#4964,#4965,#4966,#4967));
#1378=EDGE_LOOP('',(#4968,#4969,#4970,#4971));
#1379=EDGE_LOOP('',(#4972,#4973,#4974,#4975));
#1380=EDGE_LOOP('',(#4976,#4977,#4978,#4979));
#1381=EDGE_LOOP('',(#4980,#4981,#4982,#4983));
#1382=EDGE_LOOP('',(#4984,#4985,#4986,#4987,#4988,#4989,#4990,#4991,#4992,
#4993,#4994,#4995));
#1383=EDGE_LOOP('',(#4996));
#1384=EDGE_LOOP('',(#4997,#4998));
#1385=EDGE_LOOP('',(#4999,#5000,#5001,#5002,#5003,#5004,#5005,#5006));
#1386=EDGE_LOOP('',(#5007,#5008,#5009,#5010));
#1387=EDGE_LOOP('',(#5011,#5012,#5013,#5014));
#1388=EDGE_LOOP('',(#5015,#5016,#5017,#5018));
#1389=EDGE_LOOP('',(#5019,#5020,#5021,#5022));
#1390=EDGE_LOOP('',(#5023,#5024,#5025,#5026));
#1391=EDGE_LOOP('',(#5027,#5028,#5029,#5030));
#1392=EDGE_LOOP('',(#5031,#5032));
#1393=EDGE_LOOP('',(#5033,#5034,#5035,#5036,#5037,#5038,#5039,#5040));
#1394=EDGE_LOOP('',(#5041,#5042,#5043,#5044));
#1395=EDGE_LOOP('',(#5045,#5046,#5047,#5048));
#1396=EDGE_LOOP('',(#5049));
#1397=EDGE_LOOP('',(#5050));
#1398=EDGE_LOOP('',(#5051,#5052,#5053,#5054));
#1399=EDGE_LOOP('',(#5055));
#1400=EDGE_LOOP('',(#5056,#5057,#5058,#5059));
#1401=EDGE_LOOP('',(#5060,#5061,#5062,#5063));
#1402=EDGE_LOOP('',(#5064));
#1403=EDGE_LOOP('',(#5065));
#1404=EDGE_LOOP('',(#5066));
#1405=EDGE_LOOP('',(#5067));
#1406=EDGE_LOOP('',(#5068,#5069,#5070));
#1407=EDGE_LOOP('',(#5071,#5072,#5073,#5074,#5075,#5076,#5077,#5078));
#1408=EDGE_LOOP('',(#5079,#5080));
#1409=EDGE_LOOP('',(#5081,#5082));
#1410=EDGE_LOOP('',(#5083,#5084,#5085,#5086,#5087,#5088,#5089,#5090,#5091,
#5092,#5093));
#1411=EDGE_LOOP('',(#5094,#5095));
#1412=EDGE_LOOP('',(#5096,#5097,#5098,#5099,#5100,#5101,#5102,#5103,#5104,
#5105,#5106,#5107));
#1413=EDGE_LOOP('',(#5108,#5109,#5110,#5111));
#1414=EDGE_LOOP('',(#5112,#5113,#5114,#5115,#5116,#5117,#5118,#5119,#5120));
#1415=EDGE_LOOP('',(#5121));
#1416=EDGE_LOOP('',(#5122));
#1417=EDGE_LOOP('',(#5123));
#1418=EDGE_LOOP('',(#5124));
#1419=EDGE_LOOP('',(#5125));
#1420=EDGE_LOOP('',(#5126));
#1421=EDGE_LOOP('',(#5127,#5128,#5129,#5130));
#1422=EDGE_LOOP('',(#5131,#5132,#5133,#5134));
#1423=EDGE_LOOP('',(#5135,#5136,#5137,#5138));
#1424=EDGE_LOOP('',(#5139,#5140,#5141,#5142));
#1425=EDGE_LOOP('',(#5143,#5144,#5145,#5146));
#1426=EDGE_LOOP('',(#5147,#5148,#5149,#5150));
#1427=EDGE_LOOP('',(#5151,#5152,#5153,#5154,#5155,#5156));
#1428=EDGE_LOOP('',(#5157));
#1429=EDGE_LOOP('',(#5158,#5159,#5160,#5161,#5162,#5163));
#1430=EDGE_LOOP('',(#5164,#5165,#5166,#5167));
#1431=EDGE_LOOP('',(#5168,#5169,#5170,#5171));
#1432=LINE('',#8507,#1790);
#1433=LINE('',#8514,#1791);
#1434=LINE('',#8521,#1792);
#1435=LINE('',#8528,#1793);
#1436=LINE('',#8535,#1794);
#1437=LINE('',#8543,#1795);
#1438=LINE('',#8583,#1796);
#1439=LINE('',#8590,#1797);
#1440=LINE('',#8597,#1798);
#1441=LINE('',#8604,#1799);
#1442=LINE('',#8611,#1800);
#1443=LINE('',#8619,#1801);
#1444=LINE('',#8659,#1802);
#1445=LINE('',#8668,#1803);
#1446=LINE('',#8677,#1804);
#1447=LINE('',#8686,#1805);
#1448=LINE('',#8694,#1806);
#1449=LINE('',#8698,#1807);
#1450=LINE('',#8702,#1808);
#1451=LINE('',#8706,#1809);
#1452=LINE('',#8724,#1810);
#1453=LINE('',#8726,#1811);
#1454=LINE('',#8728,#1812);
#1455=LINE('',#8729,#1813);
#1456=LINE('',#8732,#1814);
#1457=LINE('',#8734,#1815);
#1458=LINE('',#8735,#1816);
#1459=LINE('',#8738,#1817);
#1460=LINE('',#8740,#1818);
#1461=LINE('',#8741,#1819);
#1462=LINE('',#8745,#1820);
#1463=LINE('',#8749,#1821);
#1464=LINE('',#8751,#1822);
#1465=LINE('',#8753,#1823);
#1466=LINE('',#8758,#1824);
#1467=LINE('',#8764,#1825);
#1468=LINE('',#8770,#1826);
#1469=LINE('',#8776,#1827);
#1470=LINE('',#8781,#1828);
#1471=LINE('',#8783,#1829);
#1472=LINE('',#8785,#1830);
#1473=LINE('',#8786,#1831);
#1474=LINE('',#8789,#1832);
#1475=LINE('',#8791,#1833);
#1476=LINE('',#8792,#1834);
#1477=LINE('',#8795,#1835);
#1478=LINE('',#8797,#1836);
#1479=LINE('',#8798,#1837);
#1480=LINE('',#8800,#1838);
#1481=LINE('',#8801,#1839);
#1482=LINE('',#8805,#1840);
#1483=LINE('',#8809,#1841);
#1484=LINE('',#8813,#1842);
#1485=LINE('',#8817,#1843);
#1486=LINE('',#8824,#1844);
#1487=LINE('',#8826,#1845);
#1488=LINE('',#8828,#1846);
#1489=LINE('',#8829,#1847);
#1490=LINE('',#8832,#1848);
#1491=LINE('',#8834,#1849);
#1492=LINE('',#8835,#1850);
#1493=LINE('',#8838,#1851);
#1494=LINE('',#8840,#1852);
#1495=LINE('',#8841,#1853);
#1496=LINE('',#8843,#1854);
#1497=LINE('',#8844,#1855);
#1498=LINE('',#8851,#1856);
#1499=LINE('',#8853,#1857);
#1500=LINE('',#8855,#1858);
#1501=LINE('',#8856,#1859);
#1502=LINE('',#8859,#1860);
#1503=LINE('',#8861,#1861);
#1504=LINE('',#8862,#1862);
#1505=LINE('',#8865,#1863);
#1506=LINE('',#8867,#1864);
#1507=LINE('',#8868,#1865);
#1508=LINE('',#8870,#1866);
#1509=LINE('',#8871,#1867);
#1510=LINE('',#8878,#1868);
#1511=LINE('',#8882,#1869);
#1512=LINE('',#8899,#1870);
#1513=LINE('',#8902,#1871);
#1514=LINE('',#8912,#1872);
#1515=LINE('',#8915,#1873);
#1516=LINE('',#8925,#1874);
#1517=LINE('',#8928,#1875);
#1518=LINE('',#8939,#1876);
#1519=LINE('',#8943,#1877);
#1520=LINE('',#8947,#1878);
#1521=LINE('',#8951,#1879);
#1522=LINE('',#8956,#1880);
#1523=LINE('',#8962,#1881);
#1524=LINE('',#8965,#1882);
#1525=LINE('',#8972,#1883);
#1526=LINE('',#8976,#1884);
#1527=LINE('',#8993,#1885);
#1528=LINE('',#8996,#1886);
#1529=LINE('',#9006,#1887);
#1530=LINE('',#9009,#1888);
#1531=LINE('',#9019,#1889);
#1532=LINE('',#9022,#1890);
#1533=LINE('',#9033,#1891);
#1534=LINE('',#9037,#1892);
#1535=LINE('',#9041,#1893);
#1536=LINE('',#9045,#1894);
#1537=LINE('',#9050,#1895);
#1538=LINE('',#9056,#1896);
#1539=LINE('',#9059,#1897);
#1540=LINE('',#9069,#1898);
#1541=LINE('',#9073,#1899);
#1542=LINE('',#9077,#1900);
#1543=LINE('',#9084,#1901);
#1544=LINE('',#9088,#1902);
#1545=LINE('',#9092,#1903);
#1546=LINE('',#9097,#1904);
#1547=LINE('',#9099,#1905);
#1548=LINE('',#9101,#1906);
#1549=LINE('',#9102,#1907);
#1550=LINE('',#9105,#1908);
#1551=LINE('',#9107,#1909);
#1552=LINE('',#9108,#1910);
#1553=LINE('',#9111,#1911);
#1554=LINE('',#9113,#1912);
#1555=LINE('',#9114,#1913);
#1556=LINE('',#9117,#1914);
#1557=LINE('',#9119,#1915);
#1558=LINE('',#9120,#1916);
#1559=LINE('',#9123,#1917);
#1560=LINE('',#9125,#1918);
#1561=LINE('',#9126,#1919);
#1562=LINE('',#9128,#1920);
#1563=LINE('',#9129,#1921);
#1564=LINE('',#9146,#1922);
#1565=LINE('',#9152,#1923);
#1566=LINE('',#9156,#1924);
#1567=LINE('',#9162,#1925);
#1568=LINE('',#9167,#1926);
#1569=LINE('',#9182,#1927);
#1570=LINE('',#9191,#1928);
#1571=LINE('',#9195,#1929);
#1572=LINE('',#9199,#1930);
#1573=LINE('',#9202,#1931);
#1574=LINE('',#9355,#1932);
#1575=LINE('',#9651,#1933);
#1576=LINE('',#9693,#1934);
#1577=LINE('',#9698,#1935);
#1578=LINE('',#9707,#1936);
#1579=LINE('',#9712,#1937);
#1580=LINE('',#9724,#1938);
#1581=LINE('',#9731,#1939);
#1582=LINE('',#9736,#1940);
#1583=LINE('',#9740,#1941);
#1584=LINE('',#9744,#1942);
#1585=LINE('',#9748,#1943);
#1586=LINE('',#9750,#1944);
#1587=LINE('',#9752,#1945);
#1588=LINE('',#9755,#1946);
#1589=LINE('',#9760,#1947);
#1590=LINE('',#9761,#1948);
#1591=LINE('',#9764,#1949);
#1592=LINE('',#9765,#1950);
#1593=LINE('',#9768,#1951);
#1594=LINE('',#9770,#1952);
#1595=LINE('',#9771,#1953);
#1596=LINE('',#9774,#1954);
#1597=LINE('',#9776,#1955);
#1598=LINE('',#9777,#1956);
#1599=LINE('',#9779,#1957);
#1600=LINE('',#9793,#1958);
#1601=LINE('',#9796,#1959);
#1602=LINE('',#9801,#1960);
#1603=LINE('',#9809,#1961);
#1604=LINE('',#9815,#1962);
#1605=LINE('',#9823,#1963);
#1606=LINE('',#9863,#1964);
#1607=LINE('',#9896,#1965);
#1608=LINE('',#9900,#1966);
#1609=LINE('',#9945,#1967);
#1610=LINE('',#9983,#1968);
#1611=LINE('',#9987,#1969);
#1612=LINE('',#9989,#1970);
#1613=LINE('',#9994,#1971);
#1614=LINE('',#9996,#1972);
#1615=LINE('',#10012,#1973);
#1616=LINE('',#10015,#1974);
#1617=LINE('',#10020,#1975);
#1618=LINE('',#10028,#1976);
#1619=LINE('',#10033,#1977);
#1620=LINE('',#10037,#1978);
#1621=LINE('',#10041,#1979);
#1622=LINE('',#10044,#1980);
#1623=LINE('',#10047,#1981);
#1624=LINE('',#10048,#1982);
#1625=LINE('',#10051,#1983);
#1626=LINE('',#10052,#1984);
#1627=LINE('',#10061,#1985);
#1628=LINE('',#10067,#1986);
#1629=LINE('',#10076,#1987);
#1630=LINE('',#10082,#1988);
#1631=LINE('',#10091,#1989);
#1632=LINE('',#10097,#1990);
#1633=LINE('',#10105,#1991);
#1634=LINE('',#10107,#1992);
#1635=LINE('',#10109,#1993);
#1636=LINE('',#10110,#1994);
#1637=LINE('',#10113,#1995);
#1638=LINE('',#10115,#1996);
#1639=LINE('',#10116,#1997);
#1640=LINE('',#10119,#1998);
#1641=LINE('',#10121,#1999);
#1642=LINE('',#10122,#2000);
#1643=LINE('',#10125,#2001);
#1644=LINE('',#10127,#2002);
#1645=LINE('',#10128,#2003);
#1646=LINE('',#10131,#2004);
#1647=LINE('',#10133,#2005);
#1648=LINE('',#10134,#2006);
#1649=LINE('',#10136,#2007);
#1650=LINE('',#10137,#2008);
#1651=LINE('',#10149,#2009);
#1652=LINE('',#10153,#2010);
#1653=LINE('',#10157,#2011);
#1654=LINE('',#10164,#2012);
#1655=LINE('',#10166,#2013);
#1656=LINE('',#10192,#2014);
#1657=LINE('',#10198,#2015);
#1658=LINE('',#10204,#2016);
#1659=LINE('',#10210,#2017);
#1660=LINE('',#10217,#2018);
#1661=LINE('',#10220,#2019);
#1662=LINE('',#10226,#2020);
#1663=LINE('',#10229,#2021);
#1664=LINE('',#10235,#2022);
#1665=LINE('',#10238,#2023);
#1666=LINE('',#10242,#2024);
#1667=LINE('',#10246,#2025);
#1668=LINE('',#10252,#2026);
#1669=LINE('',#10258,#2027);
#1670=LINE('',#10264,#2028);
#1671=LINE('',#10268,#2029);
#1672=LINE('',#10270,#2030);
#1673=LINE('',#10272,#2031);
#1674=LINE('',#10276,#2032);
#1675=LINE('',#10278,#2033);
#1676=LINE('',#10280,#2034);
#1677=LINE('',#10285,#2035);
#1678=LINE('',#10287,#2036);
#1679=LINE('',#10289,#2037);
#1680=LINE('',#10293,#2038);
#1681=LINE('',#10295,#2039);
#1682=LINE('',#10297,#2040);
#1683=LINE('',#10300,#2041);
#1684=LINE('',#10302,#2042);
#1685=LINE('',#10304,#2043);
#1686=LINE('',#10308,#2044);
#1687=LINE('',#10310,#2045);
#1688=LINE('',#10312,#2046);
#1689=LINE('',#10315,#2047);
#1690=LINE('',#10317,#2048);
#1691=LINE('',#10319,#2049);
#1692=LINE('',#10323,#2050);
#1693=LINE('',#10325,#2051);
#1694=LINE('',#10327,#2052);
#1695=LINE('',#10332,#2053);
#1696=LINE('',#10335,#2054);
#1697=LINE('',#10339,#2055);
#1698=LINE('',#10340,#2056);
#1699=LINE('',#10343,#2057);
#1700=LINE('',#10344,#2058);
#1701=LINE('',#10347,#2059);
#1702=LINE('',#10349,#2060);
#1703=LINE('',#10350,#2061);
#1704=LINE('',#10352,#2062);
#1705=LINE('',#10355,#2063);
#1706=LINE('',#10356,#2064);
#1707=LINE('',#10361,#2065);
#1708=LINE('',#10363,#2066);
#1709=LINE('',#10365,#2067);
#1710=LINE('',#10373,#2068);
#1711=LINE('',#10381,#2069);
#1712=LINE('',#10383,#2070);
#1713=LINE('',#10384,#2071);
#1714=LINE('',#10391,#2072);
#1715=LINE('',#10392,#2073);
#1716=LINE('',#10393,#2074);
#1717=LINE('',#10396,#2075);
#1718=LINE('',#10400,#2076);
#1719=LINE('',#10405,#2077);
#1720=LINE('',#10409,#2078);
#1721=LINE('',#10413,#2079);
#1722=LINE('',#10417,#2080);
#1723=LINE('',#10420,#2081);
#1724=LINE('',#10423,#2082);
#1725=LINE('',#10425,#2083);
#1726=LINE('',#10427,#2084);
#1727=LINE('',#10430,#2085);
#1728=LINE('',#10432,#2086);
#1729=LINE('',#10433,#2087);
#1730=LINE('',#10435,#2088);
#1731=LINE('',#10438,#2089);
#1732=LINE('',#10439,#2090);
#1733=LINE('',#10444,#2091);
#1734=LINE('',#10446,#2092);
#1735=LINE('',#10448,#2093);
#1736=LINE('',#10454,#2094);
#1737=LINE('',#10457,#2095);
#1738=LINE('',#10459,#2096);
#1739=LINE('',#10461,#2097);
#1740=LINE('',#10464,#2098);
#1741=LINE('',#10466,#2099);
#1742=LINE('',#10467,#2100);
#1743=LINE('',#10469,#2101);
#1744=LINE('',#10472,#2102);
#1745=LINE('',#10473,#2103);
#1746=LINE('',#10478,#2104);
#1747=LINE('',#10480,#2105);
#1748=LINE('',#10482,#2106);
#1749=LINE('',#10488,#2107);
#1750=LINE('',#10491,#2108);
#1751=LINE('',#10493,#2109);
#1752=LINE('',#10495,#2110);
#1753=LINE('',#10497,#2111);
#1754=LINE('',#10499,#2112);
#1755=LINE('',#10503,#2113);
#1756=LINE('',#10504,#2114);
#1757=LINE('',#10512,#2115);
#1758=LINE('',#10520,#2116);
#1759=LINE('',#10526,#2117);
#1760=LINE('',#10534,#2118);
#1761=LINE('',#10574,#2119);
#1762=LINE('',#10607,#2120);
#1763=LINE('',#10611,#2121);
#1764=LINE('',#10656,#2122);
#1765=LINE('',#10694,#2123);
#1766=LINE('',#10698,#2124);
#1767=LINE('',#10700,#2125);
#1768=LINE('',#10705,#2126);
#1769=LINE('',#10707,#2127);
#1770=LINE('',#10718,#2128);
#1771=LINE('',#10720,#2129);
#1772=LINE('',#10722,#2130);
#1773=LINE('',#10723,#2131);
#1774=LINE('',#10726,#2132);
#1775=LINE('',#10728,#2133);
#1776=LINE('',#10729,#2134);
#1777=LINE('',#10732,#2135);
#1778=LINE('',#10734,#2136);
#1779=LINE('',#10735,#2137);
#1780=LINE('',#10738,#2138);
#1781=LINE('',#10740,#2139);
#1782=LINE('',#10741,#2140);
#1783=LINE('',#10744,#2141);
#1784=LINE('',#10746,#2142);
#1785=LINE('',#10747,#2143);
#1786=LINE('',#10749,#2144);
#1787=LINE('',#10750,#2145);
#1788=LINE('',#10758,#2146);
#1789=LINE('',#10760,#2147);
#1790=VECTOR('',#6676,0.165);
#1791=VECTOR('',#6685,0.165);
#1792=VECTOR('',#6694,0.165);
#1793=VECTOR('',#6703,0.165);
#1794=VECTOR('',#6712,1.5);
#1795=VECTOR('',#6723,1.02);
#1796=VECTOR('',#6728,0.165);
#1797=VECTOR('',#6737,0.165);
#1798=VECTOR('',#6746,0.165);
#1799=VECTOR('',#6755,0.165);
#1800=VECTOR('',#6764,1.5);
#1801=VECTOR('',#6775,1.02);
#1802=VECTOR('',#6780,0.5);
#1803=VECTOR('',#6791,0.5);
#1804=VECTOR('',#6802,0.5);
#1805=VECTOR('',#6813,0.5);
#1806=VECTOR('',#6824,0.275);
#1807=VECTOR('',#6829,0.275);
#1808=VECTOR('',#6834,0.275);
#1809=VECTOR('',#6839,0.275);
#1810=VECTOR('',#6862,1.);
#1811=VECTOR('',#6863,1.);
#1812=VECTOR('',#6864,1.);
#1813=VECTOR('',#6865,1.);
#1814=VECTOR('',#6868,1.);
#1815=VECTOR('',#6869,1.);
#1816=VECTOR('',#6870,1.);
#1817=VECTOR('',#6873,1.);
#1818=VECTOR('',#6874,1.);
#1819=VECTOR('',#6875,1.);
#1820=VECTOR('',#6880,0.25);
#1821=VECTOR('',#6885,0.25);
#1822=VECTOR('',#6888,1.);
#1823=VECTOR('',#6891,1.);
#1824=VECTOR('',#6896,0.33);
#1825=VECTOR('',#6903,0.33);
#1826=VECTOR('',#6910,0.33);
#1827=VECTOR('',#6917,0.33);
#1828=VECTOR('',#6922,1.);
#1829=VECTOR('',#6923,1.);
#1830=VECTOR('',#6924,1.);
#1831=VECTOR('',#6925,1.);
#1832=VECTOR('',#6928,1.);
#1833=VECTOR('',#6929,1.);
#1834=VECTOR('',#6930,1.);
#1835=VECTOR('',#6933,1.);
#1836=VECTOR('',#6934,1.);
#1837=VECTOR('',#6935,1.);
#1838=VECTOR('',#6938,1.);
#1839=VECTOR('',#6939,1.);
#1840=VECTOR('',#6944,0.21);
#1841=VECTOR('',#6949,0.21);
#1842=VECTOR('',#6954,0.21);
#1843=VECTOR('',#6959,0.21);
#1844=VECTOR('',#6968,1.);
#1845=VECTOR('',#6969,1.);
#1846=VECTOR('',#6970,1.);
#1847=VECTOR('',#6971,1.);
#1848=VECTOR('',#6974,1.);
#1849=VECTOR('',#6975,1.);
#1850=VECTOR('',#6976,1.);
#1851=VECTOR('',#6979,1.);
#1852=VECTOR('',#6980,1.);
#1853=VECTOR('',#6981,1.);
#1854=VECTOR('',#6984,1.);
#1855=VECTOR('',#6985,1.);
#1856=VECTOR('',#6994,1.);
#1857=VECTOR('',#6995,1.);
#1858=VECTOR('',#6996,1.);
#1859=VECTOR('',#6997,1.);
#1860=VECTOR('',#7000,1.);
#1861=VECTOR('',#7001,1.);
#1862=VECTOR('',#7002,1.);
#1863=VECTOR('',#7005,1.);
#1864=VECTOR('',#7006,1.);
#1865=VECTOR('',#7007,1.);
#1866=VECTOR('',#7010,1.);
#1867=VECTOR('',#7011,1.);
#1868=VECTOR('',#7020,1.);
#1869=VECTOR('',#7023,1.);
#1870=VECTOR('',#7044,1.);
#1871=VECTOR('',#7047,1.);
#1872=VECTOR('',#7058,1.);
#1873=VECTOR('',#7061,1.);
#1874=VECTOR('',#7072,1.);
#1875=VECTOR('',#7075,1.);
#1876=VECTOR('',#7092,0.225);
#1877=VECTOR('',#7097,0.225);
#1878=VECTOR('',#7102,0.225);
#1879=VECTOR('',#7107,0.225);
#1880=VECTOR('',#7112,1.49);
#1881=VECTOR('',#7121,0.71);
#1882=VECTOR('',#7124,2.);
#1883=VECTOR('',#7133,1.);
#1884=VECTOR('',#7136,1.);
#1885=VECTOR('',#7157,1.);
#1886=VECTOR('',#7160,1.);
#1887=VECTOR('',#7171,1.);
#1888=VECTOR('',#7174,1.);
#1889=VECTOR('',#7185,1.);
#1890=VECTOR('',#7188,1.);
#1891=VECTOR('',#7205,0.225);
#1892=VECTOR('',#7210,0.225);
#1893=VECTOR('',#7215,0.225);
#1894=VECTOR('',#7220,0.225);
#1895=VECTOR('',#7225,1.49);
#1896=VECTOR('',#7234,0.71);
#1897=VECTOR('',#7237,2.);
#1898=VECTOR('',#7252,0.4);
#1899=VECTOR('',#7257,0.425);
#1900=VECTOR('',#7262,0.41);
#1901=VECTOR('',#7271,0.26);
#1902=VECTOR('',#7276,0.25);
#1903=VECTOR('',#7281,0.225);
#1904=VECTOR('',#7286,1.);
#1905=VECTOR('',#7287,1.);
#1906=VECTOR('',#7288,1.);
#1907=VECTOR('',#7289,1.);
#1908=VECTOR('',#7292,1.);
#1909=VECTOR('',#7293,1.);
#1910=VECTOR('',#7294,1.);
#1911=VECTOR('',#7297,1.);
#1912=VECTOR('',#7298,1.);
#1913=VECTOR('',#7299,1.);
#1914=VECTOR('',#7302,1.);
#1915=VECTOR('',#7303,1.);
#1916=VECTOR('',#7304,1.);
#1917=VECTOR('',#7307,1.);
#1918=VECTOR('',#7308,1.);
#1919=VECTOR('',#7309,1.);
#1920=VECTOR('',#7312,1.);
#1921=VECTOR('',#7313,1.);
#1922=VECTOR('',#7336,0.976185);
#1923=VECTOR('',#7343,0.5);
#1924=VECTOR('',#7348,0.53);
#1925=VECTOR('',#7357,0.976185);
#1926=VECTOR('',#7364,0.53);
#1927=VECTOR('',#7383,1.023815);
#1928=VECTOR('',#7394,1.47);
#1929=VECTOR('',#7399,1.5);
#1930=VECTOR('',#7404,1.47);
#1931=VECTOR('',#7409,1.023815);
#1932=VECTOR('',#7460,1.019052);
#1933=VECTOR('',#7537,0.980948);
#1934=VECTOR('',#7566,1.013815);
#1935=VECTOR('',#7573,0.991185);
#1936=VECTOR('',#7584,1.013815);
#1937=VECTOR('',#7591,0.991185);
#1938=VECTOR('',#7610,0.165);
#1939=VECTOR('',#7619,0.25);
#1940=VECTOR('',#7624,1.);
#1941=VECTOR('',#7627,1.);
#1942=VECTOR('',#7632,1.);
#1943=VECTOR('',#7635,1.);
#1944=VECTOR('',#7636,1.);
#1945=VECTOR('',#7637,1.);
#1946=VECTOR('',#7640,1.);
#1947=VECTOR('',#7645,1.);
#1948=VECTOR('',#7646,1.);
#1949=VECTOR('',#7649,1.);
#1950=VECTOR('',#7650,1.);
#1951=VECTOR('',#7653,1.);
#1952=VECTOR('',#7654,1.);
#1953=VECTOR('',#7655,1.);
#1954=VECTOR('',#7658,1.);
#1955=VECTOR('',#7659,1.);
#1956=VECTOR('',#7660,1.);
#1957=VECTOR('',#7663,1.);
#1958=VECTOR('',#7684,0.7);
#1959=VECTOR('',#7687,0.5);
#1960=VECTOR('',#7694,0.5);
#1961=VECTOR('',#7705,0.505);
#1962=VECTOR('',#7712,0.7);
#1963=VECTOR('',#7723,1.);
#1964=VECTOR('',#7730,0.165);
#1965=VECTOR('',#7735,1.);
#1966=VECTOR('',#7738,1.);
#1967=VECTOR('',#7743,0.165);
#1968=VECTOR('',#7748,1.);
#1969=VECTOR('',#7753,0.505);
#1970=VECTOR('',#7754,0.505);
#1971=VECTOR('',#7761,0.9);
#1972=VECTOR('',#7762,0.9);
#1973=VECTOR('',#7785,0.5);
#1974=VECTOR('',#7788,0.3);
#1975=VECTOR('',#7795,0.3);
#1976=VECTOR('',#7806,0.5);
#1977=VECTOR('',#7811,1.);
#1978=VECTOR('',#7814,1.);
#1979=VECTOR('',#7819,1.);
#1980=VECTOR('',#7822,1.);
#1981=VECTOR('',#7825,1.);
#1982=VECTOR('',#7826,1.);
#1983=VECTOR('',#7829,1.);
#1984=VECTOR('',#7830,1.);
#1985=VECTOR('',#7843,0.505);
#1986=VECTOR('',#7850,0.7);
#1987=VECTOR('',#7863,0.225);
#1988=VECTOR('',#7870,0.7);
#1989=VECTOR('',#7883,0.4);
#1990=VECTOR('',#7890,1.4);
#1991=VECTOR('',#7901,1.);
#1992=VECTOR('',#7902,1.);
#1993=VECTOR('',#7903,1.);
#1994=VECTOR('',#7904,1.);
#1995=VECTOR('',#7907,1.);
#1996=VECTOR('',#7908,1.);
#1997=VECTOR('',#7909,1.);
#1998=VECTOR('',#7912,1.);
#1999=VECTOR('',#7913,1.);
#2000=VECTOR('',#7914,1.);
#2001=VECTOR('',#7917,1.);
#2002=VECTOR('',#7918,1.);
#2003=VECTOR('',#7919,1.);
#2004=VECTOR('',#7922,1.);
#2005=VECTOR('',#7923,1.);
#2006=VECTOR('',#7924,1.);
#2007=VECTOR('',#7927,1.);
#2008=VECTOR('',#7928,1.);
#2009=VECTOR('',#7945,0.325);
#2010=VECTOR('',#7950,0.35);
#2011=VECTOR('',#7955,0.335);
#2012=VECTOR('',#7964,0.21);
#2013=VECTOR('',#7967,0.2);
#2014=VECTOR('',#8014,0.165);
#2015=VECTOR('',#8021,0.165);
#2016=VECTOR('',#8028,0.165);
#2017=VECTOR('',#8035,0.165);
#2018=VECTOR('',#8042,1.);
#2019=VECTOR('',#8045,1.);
#2020=VECTOR('',#8050,1.);
#2021=VECTOR('',#8053,1.);
#2022=VECTOR('',#8058,1.);
#2023=VECTOR('',#8061,1.);
#2024=VECTOR('',#8064,1.);
#2025=VECTOR('',#8067,1.);
#2026=VECTOR('',#8074,1.);
#2027=VECTOR('',#8081,1.);
#2028=VECTOR('',#8088,1.);
#2029=VECTOR('',#8093,1.);
#2030=VECTOR('',#8094,1.);
#2031=VECTOR('',#8095,1.);
#2032=VECTOR('',#8098,1.);
#2033=VECTOR('',#8099,1.);
#2034=VECTOR('',#8100,1.);
#2035=VECTOR('',#8105,1.);
#2036=VECTOR('',#8106,1.);
#2037=VECTOR('',#8107,1.);
#2038=VECTOR('',#8110,1.);
#2039=VECTOR('',#8111,1.);
#2040=VECTOR('',#8112,1.);
#2041=VECTOR('',#8115,1.);
#2042=VECTOR('',#8116,1.);
#2043=VECTOR('',#8117,1.);
#2044=VECTOR('',#8120,1.);
#2045=VECTOR('',#8121,1.);
#2046=VECTOR('',#8122,1.);
#2047=VECTOR('',#8125,1.);
#2048=VECTOR('',#8126,1.);
#2049=VECTOR('',#8127,1.);
#2050=VECTOR('',#8130,1.);
#2051=VECTOR('',#8131,1.);
#2052=VECTOR('',#8132,1.);
#2053=VECTOR('',#8139,1.);
#2054=VECTOR('',#8142,1.);
#2055=VECTOR('',#8147,1.);
#2056=VECTOR('',#8148,1.);
#2057=VECTOR('',#8151,1.);
#2058=VECTOR('',#8152,1.);
#2059=VECTOR('',#8155,1.);
#2060=VECTOR('',#8156,1.);
#2061=VECTOR('',#8157,1.);
#2062=VECTOR('',#8160,1.);
#2063=VECTOR('',#8163,1.);
#2064=VECTOR('',#8164,1.);
#2065=VECTOR('',#8169,1.);
#2066=VECTOR('',#8170,1.);
#2067=VECTOR('',#8171,1.);
#2068=VECTOR('',#8180,1.);
#2069=VECTOR('',#8187,1.);
#2070=VECTOR('',#8188,1.);
#2071=VECTOR('',#8189,1.);
#2072=VECTOR('',#8198,1.);
#2073=VECTOR('',#8199,1.);
#2074=VECTOR('',#8200,1.);
#2075=VECTOR('',#8203,1.);
#2076=VECTOR('',#8206,0.7);
#2077=VECTOR('',#8211,1.);
#2078=VECTOR('',#8214,1.);
#2079=VECTOR('',#8217,1.);
#2080=VECTOR('',#8220,1.);
#2081=VECTOR('',#8223,1.);
#2082=VECTOR('',#8228,1.);
#2083=VECTOR('',#8231,1.);
#2084=VECTOR('',#8234,1.);
#2085=VECTOR('',#8237,1.);
#2086=VECTOR('',#8238,1.);
#2087=VECTOR('',#8239,1.);
#2088=VECTOR('',#8242,1.);
#2089=VECTOR('',#8245,1.);
#2090=VECTOR('',#8246,1.);
#2091=VECTOR('',#8251,1.);
#2092=VECTOR('',#8252,1.);
#2093=VECTOR('',#8253,1.);
#2094=VECTOR('',#8264,1.);
#2095=VECTOR('',#8269,1.);
#2096=VECTOR('',#8272,1.);
#2097=VECTOR('',#8275,1.);
#2098=VECTOR('',#8278,1.);
#2099=VECTOR('',#8279,1.);
#2100=VECTOR('',#8280,1.);
#2101=VECTOR('',#8283,1.);
#2102=VECTOR('',#8286,1.);
#2103=VECTOR('',#8287,1.);
#2104=VECTOR('',#8292,1.);
#2105=VECTOR('',#8293,1.);
#2106=VECTOR('',#8294,1.);
#2107=VECTOR('',#8305,1.);
#2108=VECTOR('',#8310,1.);
#2109=VECTOR('',#8313,1.);
#2110=VECTOR('',#8316,1.);
#2111=VECTOR('',#8319,1.);
#2112=VECTOR('',#8322,1.);
#2113=VECTOR('',#8329,1.);
#2114=VECTOR('',#8330,1.);
#2115=VECTOR('',#8341,0.5);
#2116=VECTOR('',#8352,0.505);
#2117=VECTOR('',#8359,0.7);
#2118=VECTOR('',#8370,1.);
#2119=VECTOR('',#8377,0.165);
#2120=VECTOR('',#8382,1.);
#2121=VECTOR('',#8385,1.);
#2122=VECTOR('',#8390,0.165);
#2123=VECTOR('',#8395,1.);
#2124=VECTOR('',#8400,0.505);
#2125=VECTOR('',#8401,0.505);
#2126=VECTOR('',#8408,0.9);
#2127=VECTOR('',#8409,0.9);
#2128=VECTOR('',#8424,1.);
#2129=VECTOR('',#8425,1.);
#2130=VECTOR('',#8426,1.);
#2131=VECTOR('',#8427,1.);
#2132=VECTOR('',#8430,1.);
#2133=VECTOR('',#8431,1.);
#2134=VECTOR('',#8432,1.);
#2135=VECTOR('',#8435,1.);
#2136=VECTOR('',#8436,1.);
#2137=VECTOR('',#8437,1.);
#2138=VECTOR('',#8440,1.);
#2139=VECTOR('',#8441,1.);
#2140=VECTOR('',#8442,1.);
#2141=VECTOR('',#8445,1.);
#2142=VECTOR('',#8446,1.);
#2143=VECTOR('',#8447,1.);
#2144=VECTOR('',#8450,1.);
#2145=VECTOR('',#8451,1.);
#2146=VECTOR('',#8462,0.185);
#2147=VECTOR('',#8465,0.2);
#2148=CIRCLE('',#5932,0.165);
#2149=CIRCLE('',#5933,0.165);
#2150=CIRCLE('',#5936,0.165);
#2151=CIRCLE('',#5937,0.165);
#2152=CIRCLE('',#5940,0.165);
#2153=CIRCLE('',#5941,0.165);
#2154=CIRCLE('',#5944,0.165);
#2155=CIRCLE('',#5945,0.165);
#2156=CIRCLE('',#5948,1.5);
#2157=CIRCLE('',#5949,1.5);
#2158=CIRCLE('',#5951,1.02);
#2159=CIRCLE('',#5953,1.02);
#2160=CIRCLE('',#5955,0.165);
#2161=CIRCLE('',#5956,0.165);
#2162=CIRCLE('',#5959,0.165);
#2163=CIRCLE('',#5960,0.165);
#2164=CIRCLE('',#5963,0.165);
#2165=CIRCLE('',#5964,0.165);
#2166=CIRCLE('',#5967,0.165);
#2167=CIRCLE('',#5968,0.165);
#2168=CIRCLE('',#5971,1.5);
#2169=CIRCLE('',#5972,1.5);
#2170=CIRCLE('',#5974,1.02);
#2171=CIRCLE('',#5976,1.02);
#2172=CIRCLE('',#5978,0.5);
#2173=CIRCLE('',#5979,0.5);
#2174=CIRCLE('',#5981,0.275);
#2175=CIRCLE('',#5983,0.5);
#2176=CIRCLE('',#5984,0.5);
#2177=CIRCLE('',#5986,0.275);
#2178=CIRCLE('',#5988,0.5);
#2179=CIRCLE('',#5989,0.5);
#2180=CIRCLE('',#5991,0.275);
#2181=CIRCLE('',#5993,0.5);
#2182=CIRCLE('',#5994,0.5);
#2183=CIRCLE('',#5996,0.275);
#2184=CIRCLE('',#5998,0.275);
#2185=CIRCLE('',#6000,0.275);
#2186=CIRCLE('',#6002,0.275);
#2187=CIRCLE('',#6004,0.275);
#2188=CIRCLE('',#6006,0.21);
#2189=CIRCLE('',#6008,0.21);
#2190=CIRCLE('',#6010,0.21);
#2191=CIRCLE('',#6012,0.21);
#2192=CIRCLE('',#6019,0.25);
#2193=CIRCLE('',#6021,0.25);
#2194=CIRCLE('',#6025,0.33);
#2195=CIRCLE('',#6026,0.33);
#2196=CIRCLE('',#6028,0.33);
#2197=CIRCLE('',#6029,0.33);
#2198=CIRCLE('',#6031,0.33);
#2199=CIRCLE('',#6032,0.33);
#2200=CIRCLE('',#6034,0.33);
#2201=CIRCLE('',#6035,0.33);
#2202=CIRCLE('',#6041,0.21);
#2203=CIRCLE('',#6043,0.21);
#2204=CIRCLE('',#6045,0.21);
#2205=CIRCLE('',#6047,0.21);
#2206=CIRCLE('',#6066,0.375);
#2207=CIRCLE('',#6067,0.375);
#2208=CIRCLE('',#6069,2.);
#2209=CIRCLE('',#6070,2.);
#2210=CIRCLE('',#6071,0.225);
#2211=CIRCLE('',#6073,2.);
#2212=CIRCLE('',#6074,0.375);
#2213=CIRCLE('',#6075,0.225);
#2214=CIRCLE('',#6077,0.375);
#2215=CIRCLE('',#6079,2.);
#2216=CIRCLE('',#6080,0.375);
#2217=CIRCLE('',#6081,0.225);
#2218=CIRCLE('',#6083,0.375);
#2219=CIRCLE('',#6085,2.);
#2220=CIRCLE('',#6086,0.375);
#2221=CIRCLE('',#6087,0.225);
#2222=CIRCLE('',#6089,0.375);
#2223=CIRCLE('',#6091,2.);
#2224=CIRCLE('',#6092,2.);
#2225=CIRCLE('',#6093,2.);
#2226=CIRCLE('',#6094,2.);
#2227=CIRCLE('',#6095,0.71);
#2228=CIRCLE('',#6097,0.225);
#2229=CIRCLE('',#6099,0.225);
#2230=CIRCLE('',#6101,0.225);
#2231=CIRCLE('',#6103,0.225);
#2232=CIRCLE('',#6105,1.49);
#2233=CIRCLE('',#6106,1.49);
#2234=CIRCLE('',#6108,0.71);
#2235=CIRCLE('',#6111,2.);
#2236=CIRCLE('',#6115,0.375);
#2237=CIRCLE('',#6116,0.375);
#2238=CIRCLE('',#6118,2.);
#2239=CIRCLE('',#6119,2.);
#2240=CIRCLE('',#6120,0.225);
#2241=CIRCLE('',#6122,2.);
#2242=CIRCLE('',#6123,0.375);
#2243=CIRCLE('',#6124,0.225);
#2244=CIRCLE('',#6126,0.375);
#2245=CIRCLE('',#6128,2.);
#2246=CIRCLE('',#6129,0.375);
#2247=CIRCLE('',#6130,0.225);
#2248=CIRCLE('',#6132,0.375);
#2249=CIRCLE('',#6134,2.);
#2250=CIRCLE('',#6135,0.375);
#2251=CIRCLE('',#6136,0.225);
#2252=CIRCLE('',#6138,0.375);
#2253=CIRCLE('',#6140,2.);
#2254=CIRCLE('',#6141,2.);
#2255=CIRCLE('',#6142,2.);
#2256=CIRCLE('',#6143,2.);
#2257=CIRCLE('',#6144,0.71);
#2258=CIRCLE('',#6146,0.225);
#2259=CIRCLE('',#6148,0.225);
#2260=CIRCLE('',#6150,0.225);
#2261=CIRCLE('',#6152,0.225);
#2262=CIRCLE('',#6154,1.49);
#2263=CIRCLE('',#6155,1.49);
#2264=CIRCLE('',#6157,0.71);
#2265=CIRCLE('',#6160,2.);
#2266=CIRCLE('',#6164,0.375);
#2267=CIRCLE('',#6166,0.425);
#2268=CIRCLE('',#6168,0.425);
#2269=CIRCLE('',#6170,0.395);
#2270=CIRCLE('',#6172,0.27);
#2271=CIRCLE('',#6174,0.24505);
#2272=CIRCLE('',#6176,0.24505);
#2273=CIRCLE('',#6178,0.2);
#2274=CIRCLE('',#6191,0.976185);
#2275=CIRCLE('',#6192,0.976185);
#2276=CIRCLE('',#6193,0.247676);
#2277=CIRCLE('',#6194,0.976185);
#2278=CIRCLE('',#6195,0.976185);
#2279=CIRCLE('',#6197,0.976185);
#2280=CIRCLE('',#6199,0.5);
#2281=CIRCLE('',#6200,0.5);
#2282=CIRCLE('',#6202,0.56);
#2283=CIRCLE('',#6205,0.976185);
#2284=CIRCLE('',#6207,0.56);
#2285=CIRCLE('',#6211,1.023815);
#2286=CIRCLE('',#6212,1.023815);
#2287=CIRCLE('',#6213,0.247676);
#2288=CIRCLE('',#6214,1.023815);
#2289=CIRCLE('',#6215,1.023815);
#2290=CIRCLE('',#6217,1.023815);
#2291=CIRCLE('',#6219,1.44);
#2292=CIRCLE('',#6220,1.023815);
#2293=CIRCLE('',#6222,1.5);
#2294=CIRCLE('',#6224,1.5);
#2295=CIRCLE('',#6226,1.44);
#2296=CIRCLE('',#6231,0.23815);
#2297=CIRCLE('',#6233,0.23815);
#2298=CIRCLE('',#6235,0.23815);
#2299=CIRCLE('',#6237,0.23815);
#2300=CIRCLE('',#6239,0.23815);
#2301=CIRCLE('',#6241,0.23815);
#2302=CIRCLE('',#6243,0.23815);
#2303=CIRCLE('',#6245,0.23815);
#2304=CIRCLE('',#6248,0.243053047864041);
#2305=CIRCLE('',#6249,0.243053047864041);
#2306=CIRCLE('',#6251,1.019052);
#2307=CIRCLE('',#6252,1.019052);
#2308=CIRCLE('',#6253,1.019052);
#2309=CIRCLE('',#6254,1.019052);
#2310=CIRCLE('',#6255,1.019052);
#2311=CIRCLE('',#6256,1.019052);
#2312=CIRCLE('',#6257,1.019052);
#2313=CIRCLE('',#6258,1.019052);
#2314=CIRCLE('',#6259,1.019052);
#2315=CIRCLE('',#6261,0.980948);
#2316=CIRCLE('',#6262,0.243053047864041);
#2317=CIRCLE('',#6264,0.243053047864041);
#2318=CIRCLE('',#6266,0.980948);
#2319=CIRCLE('',#6267,0.243053047864041);
#2320=CIRCLE('',#6269,0.243053047864041);
#2321=CIRCLE('',#6271,0.980948);
#2322=CIRCLE('',#6272,0.243053047864041);
#2323=CIRCLE('',#6274,0.243053047864041);
#2324=CIRCLE('',#6276,0.980948);
#2325=CIRCLE('',#6277,0.243053047864041);
#2326=CIRCLE('',#6279,0.243053047864041);
#2327=CIRCLE('',#6281,0.980948);
#2328=CIRCLE('',#6282,0.243053047864041);
#2329=CIRCLE('',#6284,0.243053047864041);
#2330=CIRCLE('',#6286,0.980948);
#2331=CIRCLE('',#6287,0.243053047864041);
#2332=CIRCLE('',#6289,0.243053047864041);
#2333=CIRCLE('',#6291,0.980948);
#2334=CIRCLE('',#6292,0.980948);
#2335=CIRCLE('',#6293,0.980948);
#2336=CIRCLE('',#6295,0.243053047864041);
#2337=CIRCLE('',#6297,0.243053047864041);
#2338=CIRCLE('',#6302,1.013815);
#2339=CIRCLE('',#6303,0.991185);
#2340=CIRCLE('',#6305,1.013815);
#2341=CIRCLE('',#6307,0.991185);
#2342=CIRCLE('',#6310,1.013815);
#2343=CIRCLE('',#6311,0.991185);
#2344=CIRCLE('',#6313,1.013815);
#2345=CIRCLE('',#6315,0.991185);
#2346=CIRCLE('',#6325,0.165);
#2347=CIRCLE('',#6326,0.165);
#2348=CIRCLE('',#6329,0.25);
#2349=CIRCLE('',#6330,0.25);
#2350=CIRCLE('',#6332,0.5);
#2351=CIRCLE('',#6333,0.5);
#2352=CIRCLE('',#6335,1.);
#2353=CIRCLE('',#6336,1.);
#2354=CIRCLE('',#6337,0.7);
#2355=CIRCLE('',#6344,1.);
#2356=CIRCLE('',#6345,1.);
#2357=CIRCLE('',#6346,0.5);
#2358=CIRCLE('',#6350,0.7);
#2359=CIRCLE('',#6351,0.5);
#2360=CIRCLE('',#6354,0.5);
#2361=CIRCLE('',#6356,0.5);
#2362=CIRCLE('',#6361,0.505);
#2363=CIRCLE('',#6362,0.505);
#2364=CIRCLE('',#6364,0.7);
#2365=CIRCLE('',#6365,0.7);
#2366=CIRCLE('',#6370,0.165);
#2367=CIRCLE('',#6371,0.165);
#2368=CIRCLE('',#6373,0.165);
#2369=CIRCLE('',#6376,0.165);
#2370=CIRCLE('',#6378,0.165);
#2371=CIRCLE('',#6381,0.505);
#2372=CIRCLE('',#6382,0.505);
#2373=CIRCLE('',#6384,0.9);
#2374=CIRCLE('',#6385,0.9);
#2375=CIRCLE('',#6390,0.5);
#2376=CIRCLE('',#6391,0.3);
#2377=CIRCLE('',#6393,0.5);
#2378=CIRCLE('',#6394,0.3);
#2379=CIRCLE('',#6397,0.3);
#2380=CIRCLE('',#6399,0.3);
#2381=CIRCLE('',#6404,0.5);
#2382=CIRCLE('',#6405,0.5);
#2383=CIRCLE('',#6407,0.6);
#2384=CIRCLE('',#6408,0.6);
#2385=CIRCLE('',#6410,1.8);
#2386=CIRCLE('',#6414,1.8);
#2387=CIRCLE('',#6418,0.505);
#2388=CIRCLE('',#6419,0.505);
#2389=CIRCLE('',#6421,0.7);
#2390=CIRCLE('',#6422,0.7);
#2391=CIRCLE('',#6427,0.225);
#2392=CIRCLE('',#6428,0.225);
#2393=CIRCLE('',#6430,0.7);
#2394=CIRCLE('',#6431,0.7);
#2395=CIRCLE('',#6436,0.4);
#2396=CIRCLE('',#6437,0.4);
#2397=CIRCLE('',#6439,1.4);
#2398=CIRCLE('',#6440,1.4);
#2399=CIRCLE('',#6453,0.1954);
#2400=CIRCLE('',#6455,0.3);
#2401=CIRCLE('',#6457,0.35);
#2402=CIRCLE('',#6459,0.35);
#2403=CIRCLE('',#6461,0.32);
#2404=CIRCLE('',#6463,0.22);
#2405=CIRCLE('',#6465,0.1954);
#2406=CIRCLE('',#6489,0.165);
#2407=CIRCLE('',#6490,0.165);
#2408=CIRCLE('',#6492,0.165);
#2409=CIRCLE('',#6493,0.165);
#2410=CIRCLE('',#6495,0.165);
#2411=CIRCLE('',#6496,0.165);
#2412=CIRCLE('',#6498,0.165);
#2413=CIRCLE('',#6499,0.165);
#2414=CIRCLE('',#6501,1.82);
#2415=CIRCLE('',#6502,1.82);
#2416=CIRCLE('',#6504,1.82);
#2417=CIRCLE('',#6505,1.82);
#2418=CIRCLE('',#6507,1.82);
#2419=CIRCLE('',#6508,1.82);
#2420=CIRCLE('',#6510,1.82);
#2421=CIRCLE('',#6511,1.82);
#2422=CIRCLE('',#6513,3.);
#2423=CIRCLE('',#6514,3.);
#2424=CIRCLE('',#6516,3.);
#2425=CIRCLE('',#6517,3.);
#2426=CIRCLE('',#6519,3.);
#2427=CIRCLE('',#6520,3.);
#2428=CIRCLE('',#6522,0.32);
#2429=CIRCLE('',#6523,3.);
#2430=CIRCLE('',#6524,3.);
#2431=CIRCLE('',#6525,0.32);
#2432=CIRCLE('',#6526,3.);
#2433=CIRCLE('',#6527,0.32);
#2434=CIRCLE('',#6528,3.);
#2435=CIRCLE('',#6529,0.32);
#2436=CIRCLE('',#6530,3.);
#2437=CIRCLE('',#6532,3.);
#2438=CIRCLE('',#6534,3.);
#2439=CIRCLE('',#6541,3.);
#2440=CIRCLE('',#6542,0.32);
#2441=CIRCLE('',#6543,0.7);
#2442=CIRCLE('',#6544,0.32);
#2443=CIRCLE('',#6546,0.32);
#2444=CIRCLE('',#6547,0.7);
#2445=CIRCLE('',#6548,0.32);
#2446=CIRCLE('',#6550,0.7);
#2447=CIRCLE('',#6551,0.32);
#2448=CIRCLE('',#6554,0.7);
#2449=CIRCLE('',#6555,0.7);
#2450=CIRCLE('',#6556,0.7);
#2451=CIRCLE('',#6557,0.7);
#2452=CIRCLE('',#6558,0.7);
#2453=CIRCLE('',#6559,0.7);
#2454=CIRCLE('',#6560,0.7);
#2455=CIRCLE('',#6569,3.);
#2456=CIRCLE('',#6570,0.32);
#2457=CIRCLE('',#6571,0.32);
#2458=CIRCLE('',#6573,0.32);
#2459=CIRCLE('',#6583,3.);
#2460=CIRCLE('',#6584,0.32);
#2461=CIRCLE('',#6585,0.32);
#2462=CIRCLE('',#6587,0.32);
#2463=CIRCLE('',#6596,0.32);
#2464=CIRCLE('',#6601,0.5);
#2465=CIRCLE('',#6603,0.5);
#2466=CIRCLE('',#6607,0.505);
#2467=CIRCLE('',#6608,0.505);
#2468=CIRCLE('',#6610,0.7);
#2469=CIRCLE('',#6611,0.7);
#2470=CIRCLE('',#6616,0.165);
#2471=CIRCLE('',#6617,0.165);
#2472=CIRCLE('',#6619,0.165);
#2473=CIRCLE('',#6622,0.165);
#2474=CIRCLE('',#6624,0.165);
#2475=CIRCLE('',#6627,0.505);
#2476=CIRCLE('',#6628,0.505);
#2477=CIRCLE('',#6630,0.9);
#2478=CIRCLE('',#6631,0.9);
#2479=CIRCLE('',#6636,0.1954);
#2480=CIRCLE('',#6645,0.17);
#2481=CIRCLE('',#6647,0.1954);
#2482=VERTEX_POINT('',#8504);
#2483=VERTEX_POINT('',#8506);
#2484=VERTEX_POINT('',#8511);
#2485=VERTEX_POINT('',#8513);
#2486=VERTEX_POINT('',#8518);
#2487=VERTEX_POINT('',#8520);
#2488=VERTEX_POINT('',#8525);
#2489=VERTEX_POINT('',#8527);
#2490=VERTEX_POINT('',#8532);
#2491=VERTEX_POINT('',#8534);
#2492=VERTEX_POINT('',#8538);
#2493=VERTEX_POINT('',#8541);
#2494=VERTEX_POINT('',#8544);
#2495=VERTEX_POINT('',#8580);
#2496=VERTEX_POINT('',#8582);
#2497=VERTEX_POINT('',#8587);
#2498=VERTEX_POINT('',#8589);
#2499=VERTEX_POINT('',#8594);
#2500=VERTEX_POINT('',#8596);
#2501=VERTEX_POINT('',#8601);
#2502=VERTEX_POINT('',#8603);
#2503=VERTEX_POINT('',#8608);
#2504=VERTEX_POINT('',#8610);
#2505=VERTEX_POINT('',#8614);
#2506=VERTEX_POINT('',#8617);
#2507=VERTEX_POINT('',#8620);
#2508=VERTEX_POINT('',#8656);
#2509=VERTEX_POINT('',#8658);
#2510=VERTEX_POINT('',#8662);
#2511=VERTEX_POINT('',#8665);
#2512=VERTEX_POINT('',#8667);
#2513=VERTEX_POINT('',#8671);
#2514=VERTEX_POINT('',#8674);
#2515=VERTEX_POINT('',#8676);
#2516=VERTEX_POINT('',#8680);
#2517=VERTEX_POINT('',#8683);
#2518=VERTEX_POINT('',#8685);
#2519=VERTEX_POINT('',#8689);
#2520=VERTEX_POINT('',#8692);
#2521=VERTEX_POINT('',#8696);
#2522=VERTEX_POINT('',#8700);
#2523=VERTEX_POINT('',#8704);
#2524=VERTEX_POINT('',#8708);
#2525=VERTEX_POINT('',#8711);
#2526=VERTEX_POINT('',#8714);
#2527=VERTEX_POINT('',#8717);
#2528=VERTEX_POINT('',#8722);
#2529=VERTEX_POINT('',#8723);
#2530=VERTEX_POINT('',#8725);
#2531=VERTEX_POINT('',#8727);
#2532=VERTEX_POINT('',#8731);
#2533=VERTEX_POINT('',#8733);
#2534=VERTEX_POINT('',#8737);
#2535=VERTEX_POINT('',#8739);
#2536=VERTEX_POINT('',#8743);
#2537=VERTEX_POINT('',#8747);
#2538=VERTEX_POINT('',#8755);
#2539=VERTEX_POINT('',#8757);
#2540=VERTEX_POINT('',#8761);
#2541=VERTEX_POINT('',#8763);
#2542=VERTEX_POINT('',#8767);
#2543=VERTEX_POINT('',#8769);
#2544=VERTEX_POINT('',#8773);
#2545=VERTEX_POINT('',#8775);
#2546=VERTEX_POINT('',#8779);
#2547=VERTEX_POINT('',#8780);
#2548=VERTEX_POINT('',#8782);
#2549=VERTEX_POINT('',#8784);
#2550=VERTEX_POINT('',#8788);
#2551=VERTEX_POINT('',#8790);
#2552=VERTEX_POINT('',#8794);
#2553=VERTEX_POINT('',#8796);
#2554=VERTEX_POINT('',#8803);
#2555=VERTEX_POINT('',#8807);
#2556=VERTEX_POINT('',#8811);
#2557=VERTEX_POINT('',#8815);
#2558=VERTEX_POINT('',#8822);
#2559=VERTEX_POINT('',#8823);
#2560=VERTEX_POINT('',#8825);
#2561=VERTEX_POINT('',#8827);
#2562=VERTEX_POINT('',#8831);
#2563=VERTEX_POINT('',#8833);
#2564=VERTEX_POINT('',#8837);
#2565=VERTEX_POINT('',#8839);
#2566=VERTEX_POINT('',#8849);
#2567=VERTEX_POINT('',#8850);
#2568=VERTEX_POINT('',#8852);
#2569=VERTEX_POINT('',#8854);
#2570=VERTEX_POINT('',#8858);
#2571=VERTEX_POINT('',#8860);
#2572=VERTEX_POINT('',#8864);
#2573=VERTEX_POINT('',#8866);
#2574=VERTEX_POINT('',#8876);
#2575=VERTEX_POINT('',#8877);
#2576=VERTEX_POINT('',#8879);
#2577=VERTEX_POINT('',#8881);
#2578=VERTEX_POINT('',#8885);
#2579=VERTEX_POINT('',#8888);
#2580=VERTEX_POINT('',#8891);
#2581=VERTEX_POINT('',#8892);
#2582=VERTEX_POINT('',#8895);
#2583=VERTEX_POINT('',#8898);
#2584=VERTEX_POINT('',#8900);
#2585=VERTEX_POINT('',#8904);
#2586=VERTEX_POINT('',#8905);
#2587=VERTEX_POINT('',#8908);
#2588=VERTEX_POINT('',#8911);
#2589=VERTEX_POINT('',#8913);
#2590=VERTEX_POINT('',#8917);
#2591=VERTEX_POINT('',#8918);
#2592=VERTEX_POINT('',#8921);
#2593=VERTEX_POINT('',#8924);
#2594=VERTEX_POINT('',#8926);
#2595=VERTEX_POINT('',#8934);
#2596=VERTEX_POINT('',#8937);
#2597=VERTEX_POINT('',#8941);
#2598=VERTEX_POINT('',#8945);
#2599=VERTEX_POINT('',#8949);
#2600=VERTEX_POINT('',#8953);
#2601=VERTEX_POINT('',#8955);
#2602=VERTEX_POINT('',#8959);
#2603=VERTEX_POINT('',#8964);
#2604=VERTEX_POINT('',#8970);
#2605=VERTEX_POINT('',#8971);
#2606=VERTEX_POINT('',#8973);
#2607=VERTEX_POINT('',#8975);
#2608=VERTEX_POINT('',#8979);
#2609=VERTEX_POINT('',#8982);
#2610=VERTEX_POINT('',#8985);
#2611=VERTEX_POINT('',#8986);
#2612=VERTEX_POINT('',#8989);
#2613=VERTEX_POINT('',#8992);
#2614=VERTEX_POINT('',#8994);
#2615=VERTEX_POINT('',#8998);
#2616=VERTEX_POINT('',#8999);
#2617=VERTEX_POINT('',#9002);
#2618=VERTEX_POINT('',#9005);
#2619=VERTEX_POINT('',#9007);
#2620=VERTEX_POINT('',#9011);
#2621=VERTEX_POINT('',#9012);
#2622=VERTEX_POINT('',#9015);
#2623=VERTEX_POINT('',#9018);
#2624=VERTEX_POINT('',#9020);
#2625=VERTEX_POINT('',#9028);
#2626=VERTEX_POINT('',#9031);
#2627=VERTEX_POINT('',#9035);
#2628=VERTEX_POINT('',#9039);
#2629=VERTEX_POINT('',#9043);
#2630=VERTEX_POINT('',#9047);
#2631=VERTEX_POINT('',#9049);
#2632=VERTEX_POINT('',#9053);
#2633=VERTEX_POINT('',#9058);
#2634=VERTEX_POINT('',#9064);
#2635=VERTEX_POINT('',#9067);
#2636=VERTEX_POINT('',#9071);
#2637=VERTEX_POINT('',#9075);
#2638=VERTEX_POINT('',#9079);
#2639=VERTEX_POINT('',#9082);
#2640=VERTEX_POINT('',#9086);
#2641=VERTEX_POINT('',#9090);
#2642=VERTEX_POINT('',#9095);
#2643=VERTEX_POINT('',#9096);
#2644=VERTEX_POINT('',#9098);
#2645=VERTEX_POINT('',#9100);
#2646=VERTEX_POINT('',#9104);
#2647=VERTEX_POINT('',#9106);
#2648=VERTEX_POINT('',#9110);
#2649=VERTEX_POINT('',#9112);
#2650=VERTEX_POINT('',#9116);
#2651=VERTEX_POINT('',#9118);
#2652=VERTEX_POINT('',#9122);
#2653=VERTEX_POINT('',#9124);
#2654=VERTEX_POINT('',#9135);
#2655=VERTEX_POINT('',#9136);
#2656=VERTEX_POINT('',#9139);
#2657=VERTEX_POINT('',#9141);
#2658=VERTEX_POINT('',#9145);
#2659=VERTEX_POINT('',#9149);
#2660=VERTEX_POINT('',#9151);
#2661=VERTEX_POINT('',#9155);
#2662=VERTEX_POINT('',#9160);
#2663=VERTEX_POINT('',#9164);
#2664=VERTEX_POINT('',#9170);
#2665=VERTEX_POINT('',#9171);
#2666=VERTEX_POINT('',#9174);
#2667=VERTEX_POINT('',#9176);
#2668=VERTEX_POINT('',#9180);
#2669=VERTEX_POINT('',#9184);
#2670=VERTEX_POINT('',#9186);
#2671=VERTEX_POINT('',#9189);
#2672=VERTEX_POINT('',#9193);
#2673=VERTEX_POINT('',#9197);
#2674=VERTEX_POINT('',#9205);
#2675=VERTEX_POINT('',#9206);
#2676=VERTEX_POINT('',#9209);
#2677=VERTEX_POINT('',#9210);
#2678=VERTEX_POINT('',#9213);
#2679=VERTEX_POINT('',#9214);
#2680=VERTEX_POINT('',#9217);
#2681=VERTEX_POINT('',#9218);
#2682=VERTEX_POINT('',#9221);
#2683=VERTEX_POINT('',#9222);
#2684=VERTEX_POINT('',#9225);
#2685=VERTEX_POINT('',#9226);
#2686=VERTEX_POINT('',#9229);
#2687=VERTEX_POINT('',#9230);
#2688=VERTEX_POINT('',#9233);
#2689=VERTEX_POINT('',#9234);
#2690=VERTEX_POINT('',#9238);
#2691=VERTEX_POINT('',#9239);
#2692=VERTEX_POINT('',#9262);
#2693=VERTEX_POINT('',#9264);
#2694=VERTEX_POINT('',#9289);
#2695=VERTEX_POINT('',#9291);
#2696=VERTEX_POINT('',#9314);
#2697=VERTEX_POINT('',#9316);
#2698=VERTEX_POINT('',#9339);
#2699=VERTEX_POINT('',#9341);
#2700=VERTEX_POINT('',#9354);
#2701=VERTEX_POINT('',#9357);
#2702=VERTEX_POINT('',#9370);
#2703=VERTEX_POINT('',#9372);
#2704=VERTEX_POINT('',#9395);
#2705=VERTEX_POINT('',#9397);
#2706=VERTEX_POINT('',#9420);
#2707=VERTEX_POINT('',#9422);
#2708=VERTEX_POINT('',#9445);
#2709=VERTEX_POINT('',#9447);
#2710=VERTEX_POINT('',#9472);
#2711=VERTEX_POINT('',#9476);
#2712=VERTEX_POINT('',#9501);
#2713=VERTEX_POINT('',#9505);
#2714=VERTEX_POINT('',#9530);
#2715=VERTEX_POINT('',#9534);
#2716=VERTEX_POINT('',#9535);
#2717=VERTEX_POINT('',#9562);
#2718=VERTEX_POINT('',#9566);
#2719=VERTEX_POINT('',#9591);
#2720=VERTEX_POINT('',#9595);
#2721=VERTEX_POINT('',#9620);
#2722=VERTEX_POINT('',#9624);
#2723=VERTEX_POINT('',#9649);
#2724=VERTEX_POINT('',#9652);
#2725=VERTEX_POINT('',#9654);
#2726=VERTEX_POINT('',#9686);
#2727=VERTEX_POINT('',#9688);
#2728=VERTEX_POINT('',#9691);
#2729=VERTEX_POINT('',#9695);
#2730=VERTEX_POINT('',#9700);
#2731=VERTEX_POINT('',#9702);
#2732=VERTEX_POINT('',#9705);
#2733=VERTEX_POINT('',#9709);
#2734=VERTEX_POINT('',#9721);
#2735=VERTEX_POINT('',#9723);
#2736=VERTEX_POINT('',#9728);
#2737=VERTEX_POINT('',#9730);
#2738=VERTEX_POINT('',#9734);
#2739=VERTEX_POINT('',#9735);
#2740=VERTEX_POINT('',#9737);
#2741=VERTEX_POINT('',#9739);
#2742=VERTEX_POINT('',#9743);
#2743=VERTEX_POINT('',#9745);
#2744=VERTEX_POINT('',#9747);
#2745=VERTEX_POINT('',#9749);
#2746=VERTEX_POINT('',#9751);
#2747=VERTEX_POINT('',#9753);
#2748=VERTEX_POINT('',#9756);
#2749=VERTEX_POINT('',#9759);
#2750=VERTEX_POINT('',#9763);
#2751=VERTEX_POINT('',#9767);
#2752=VERTEX_POINT('',#9769);
#2753=VERTEX_POINT('',#9773);
#2754=VERTEX_POINT('',#9775);
#2755=VERTEX_POINT('',#9783);
#2756=VERTEX_POINT('',#9788);
#2757=VERTEX_POINT('',#9790);
#2758=VERTEX_POINT('',#9795);
#2759=VERTEX_POINT('',#9799);
#2760=VERTEX_POINT('',#9806);
#2761=VERTEX_POINT('',#9808);
#2762=VERTEX_POINT('',#9812);
#2763=VERTEX_POINT('',#9814);
#2764=VERTEX_POINT('',#9821);
#2765=VERTEX_POINT('',#9822);
#2766=VERTEX_POINT('',#9824);
#2767=VERTEX_POINT('',#9828);
#2768=VERTEX_POINT('',#9864);
#2769=VERTEX_POINT('',#9879);
#2770=VERTEX_POINT('',#9898);
#2771=VERTEX_POINT('',#9899);
#2772=VERTEX_POINT('',#9903);
#2773=VERTEX_POINT('',#9904);
#2774=VERTEX_POINT('',#9915);
#2775=VERTEX_POINT('',#9944);
#2776=VERTEX_POINT('',#9946);
#2777=VERTEX_POINT('',#9955);
#2778=VERTEX_POINT('',#9957);
#2779=VERTEX_POINT('',#9985);
#2780=VERTEX_POINT('',#9988);
#2781=VERTEX_POINT('',#9992);
#2782=VERTEX_POINT('',#9995);
#2783=VERTEX_POINT('',#10002);
#2784=VERTEX_POINT('',#10004);
#2785=VERTEX_POINT('',#10007);
#2786=VERTEX_POINT('',#10009);
#2787=VERTEX_POINT('',#10014);
#2788=VERTEX_POINT('',#10018);
#2789=VERTEX_POINT('',#10025);
#2790=VERTEX_POINT('',#10027);
#2791=VERTEX_POINT('',#10031);
#2792=VERTEX_POINT('',#10032);
#2793=VERTEX_POINT('',#10034);
#2794=VERTEX_POINT('',#10036);
#2795=VERTEX_POINT('',#10040);
#2796=VERTEX_POINT('',#10042);
#2797=VERTEX_POINT('',#10046);
#2798=VERTEX_POINT('',#10050);
#2799=VERTEX_POINT('',#10058);
#2800=VERTEX_POINT('',#10060);
#2801=VERTEX_POINT('',#10064);
#2802=VERTEX_POINT('',#10066);
#2803=VERTEX_POINT('',#10073);
#2804=VERTEX_POINT('',#10075);
#2805=VERTEX_POINT('',#10079);
#2806=VERTEX_POINT('',#10081);
#2807=VERTEX_POINT('',#10088);
#2808=VERTEX_POINT('',#10090);
#2809=VERTEX_POINT('',#10094);
#2810=VERTEX_POINT('',#10096);
#2811=VERTEX_POINT('',#10103);
#2812=VERTEX_POINT('',#10104);
#2813=VERTEX_POINT('',#10106);
#2814=VERTEX_POINT('',#10108);
#2815=VERTEX_POINT('',#10112);
#2816=VERTEX_POINT('',#10114);
#2817=VERTEX_POINT('',#10118);
#2818=VERTEX_POINT('',#10120);
#2819=VERTEX_POINT('',#10124);
#2820=VERTEX_POINT('',#10126);
#2821=VERTEX_POINT('',#10130);
#2822=VERTEX_POINT('',#10132);
#2823=VERTEX_POINT('',#10141);
#2824=VERTEX_POINT('',#10144);
#2825=VERTEX_POINT('',#10147);
#2826=VERTEX_POINT('',#10151);
#2827=VERTEX_POINT('',#10155);
#2828=VERTEX_POINT('',#10159);
#2829=VERTEX_POINT('',#10162);
#2830=VERTEX_POINT('',#10189);
#2831=VERTEX_POINT('',#10191);
#2832=VERTEX_POINT('',#10195);
#2833=VERTEX_POINT('',#10197);
#2834=VERTEX_POINT('',#10201);
#2835=VERTEX_POINT('',#10203);
#2836=VERTEX_POINT('',#10207);
#2837=VERTEX_POINT('',#10209);
#2838=VERTEX_POINT('',#10213);
#2839=VERTEX_POINT('',#10214);
#2840=VERTEX_POINT('',#10216);
#2841=VERTEX_POINT('',#10218);
#2842=VERTEX_POINT('',#10222);
#2843=VERTEX_POINT('',#10223);
#2844=VERTEX_POINT('',#10225);
#2845=VERTEX_POINT('',#10227);
#2846=VERTEX_POINT('',#10231);
#2847=VERTEX_POINT('',#10232);
#2848=VERTEX_POINT('',#10234);
#2849=VERTEX_POINT('',#10236);
#2850=VERTEX_POINT('',#10240);
#2851=VERTEX_POINT('',#10241);
#2852=VERTEX_POINT('',#10243);
#2853=VERTEX_POINT('',#10245);
#2854=VERTEX_POINT('',#10249);
#2855=VERTEX_POINT('',#10251);
#2856=VERTEX_POINT('',#10255);
#2857=VERTEX_POINT('',#10257);
#2858=VERTEX_POINT('',#10261);
#2859=VERTEX_POINT('',#10263);
#2860=VERTEX_POINT('',#10267);
#2861=VERTEX_POINT('',#10269);
#2862=VERTEX_POINT('',#10271);
#2863=VERTEX_POINT('',#10273);
#2864=VERTEX_POINT('',#10275);
#2865=VERTEX_POINT('',#10277);
#2866=VERTEX_POINT('',#10279);
#2867=VERTEX_POINT('',#10282);
#2868=VERTEX_POINT('',#10284);
#2869=VERTEX_POINT('',#10286);
#2870=VERTEX_POINT('',#10288);
#2871=VERTEX_POINT('',#10290);
#2872=VERTEX_POINT('',#10292);
#2873=VERTEX_POINT('',#10294);
#2874=VERTEX_POINT('',#10296);
#2875=VERTEX_POINT('',#10299);
#2876=VERTEX_POINT('',#10301);
#2877=VERTEX_POINT('',#10303);
#2878=VERTEX_POINT('',#10305);
#2879=VERTEX_POINT('',#10307);
#2880=VERTEX_POINT('',#10309);
#2881=VERTEX_POINT('',#10311);
#2882=VERTEX_POINT('',#10314);
#2883=VERTEX_POINT('',#10316);
#2884=VERTEX_POINT('',#10318);
#2885=VERTEX_POINT('',#10320);
#2886=VERTEX_POINT('',#10322);
#2887=VERTEX_POINT('',#10324);
#2888=VERTEX_POINT('',#10326);
#2889=VERTEX_POINT('',#10330);
#2890=VERTEX_POINT('',#10334);
#2891=VERTEX_POINT('',#10338);
#2892=VERTEX_POINT('',#10342);
#2893=VERTEX_POINT('',#10346);
#2894=VERTEX_POINT('',#10348);
#2895=VERTEX_POINT('',#10354);
#2896=VERTEX_POINT('',#10358);
#2897=VERTEX_POINT('',#10360);
#2898=VERTEX_POINT('',#10362);
#2899=VERTEX_POINT('',#10364);
#2900=VERTEX_POINT('',#10366);
#2901=VERTEX_POINT('',#10368);
#2902=VERTEX_POINT('',#10372);
#2903=VERTEX_POINT('',#10374);
#2904=VERTEX_POINT('',#10376);
#2905=VERTEX_POINT('',#10378);
#2906=VERTEX_POINT('',#10380);
#2907=VERTEX_POINT('',#10382);
#2908=VERTEX_POINT('',#10386);
#2909=VERTEX_POINT('',#10387);
#2910=VERTEX_POINT('',#10395);
#2911=VERTEX_POINT('',#10397);
#2912=VERTEX_POINT('',#10399);
#2913=VERTEX_POINT('',#10402);
#2914=VERTEX_POINT('',#10404);
#2915=VERTEX_POINT('',#10406);
#2916=VERTEX_POINT('',#10408);
#2917=VERTEX_POINT('',#10410);
#2918=VERTEX_POINT('',#10412);
#2919=VERTEX_POINT('',#10414);
#2920=VERTEX_POINT('',#10416);
#2921=VERTEX_POINT('',#10418);
#2922=VERTEX_POINT('',#10429);
#2923=VERTEX_POINT('',#10431);
#2924=VERTEX_POINT('',#10437);
#2925=VERTEX_POINT('',#10441);
#2926=VERTEX_POINT('',#10443);
#2927=VERTEX_POINT('',#10445);
#2928=VERTEX_POINT('',#10447);
#2929=VERTEX_POINT('',#10463);
#2930=VERTEX_POINT('',#10465);
#2931=VERTEX_POINT('',#10471);
#2932=VERTEX_POINT('',#10475);
#2933=VERTEX_POINT('',#10477);
#2934=VERTEX_POINT('',#10479);
#2935=VERTEX_POINT('',#10481);
#2936=VERTEX_POINT('',#10508);
#2937=VERTEX_POINT('',#10511);
#2938=VERTEX_POINT('',#10517);
#2939=VERTEX_POINT('',#10519);
#2940=VERTEX_POINT('',#10523);
#2941=VERTEX_POINT('',#10525);
#2942=VERTEX_POINT('',#10532);
#2943=VERTEX_POINT('',#10533);
#2944=VERTEX_POINT('',#10535);
#2945=VERTEX_POINT('',#10539);
#2946=VERTEX_POINT('',#10575);
#2947=VERTEX_POINT('',#10590);
#2948=VERTEX_POINT('',#10609);
#2949=VERTEX_POINT('',#10610);
#2950=VERTEX_POINT('',#10614);
#2951=VERTEX_POINT('',#10615);
#2952=VERTEX_POINT('',#10626);
#2953=VERTEX_POINT('',#10655);
#2954=VERTEX_POINT('',#10657);
#2955=VERTEX_POINT('',#10666);
#2956=VERTEX_POINT('',#10668);
#2957=VERTEX_POINT('',#10696);
#2958=VERTEX_POINT('',#10699);
#2959=VERTEX_POINT('',#10703);
#2960=VERTEX_POINT('',#10706);
#2961=VERTEX_POINT('',#10713);
#2962=VERTEX_POINT('',#10716);
#2963=VERTEX_POINT('',#10717);
#2964=VERTEX_POINT('',#10719);
#2965=VERTEX_POINT('',#10721);
#2966=VERTEX_POINT('',#10725);
#2967=VERTEX_POINT('',#10727);
#2968=VERTEX_POINT('',#10731);
#2969=VERTEX_POINT('',#10733);
#2970=VERTEX_POINT('',#10737);
#2971=VERTEX_POINT('',#10739);
#2972=VERTEX_POINT('',#10743);
#2973=VERTEX_POINT('',#10745);
#2974=VERTEX_POINT('',#10753);
#2975=VERTEX_POINT('',#10756);
#2976=EDGE_CURVE('',#2482,#2482,#2148,.T.);
#2977=EDGE_CURVE('',#2482,#2483,#1432,.T.);
#2978=EDGE_CURVE('',#2483,#2483,#2149,.T.);
#2979=EDGE_CURVE('',#2484,#2484,#2150,.T.);
#2980=EDGE_CURVE('',#2484,#2485,#1433,.T.);
#2981=EDGE_CURVE('',#2485,#2485,#2151,.T.);
#2982=EDGE_CURVE('',#2486,#2486,#2152,.T.);
#2983=EDGE_CURVE('',#2486,#2487,#1434,.T.);
#2984=EDGE_CURVE('',#2487,#2487,#2153,.T.);
#2985=EDGE_CURVE('',#2488,#2488,#2154,.T.);
#2986=EDGE_CURVE('',#2488,#2489,#1435,.T.);
#2987=EDGE_CURVE('',#2489,#2489,#2155,.T.);
#2988=EDGE_CURVE('',#2490,#2490,#2156,.T.);
#2989=EDGE_CURVE('',#2490,#2491,#1436,.T.);
#2990=EDGE_CURVE('',#2491,#2491,#2157,.T.);
#2991=EDGE_CURVE('',#2492,#2492,#2158,.T.);
#2992=EDGE_CURVE('',#2493,#2493,#2159,.T.);
#2993=EDGE_CURVE('',#2493,#2492,#1437,.T.);
#2994=EDGE_CURVE('',#2494,#2494,#319,.T.);
#2995=EDGE_CURVE('',#2495,#2495,#2160,.T.);
#2996=EDGE_CURVE('',#2495,#2496,#1438,.T.);
#2997=EDGE_CURVE('',#2496,#2496,#2161,.T.);
#2998=EDGE_CURVE('',#2497,#2497,#2162,.T.);
#2999=EDGE_CURVE('',#2497,#2498,#1439,.T.);
#3000=EDGE_CURVE('',#2498,#2498,#2163,.T.);
#3001=EDGE_CURVE('',#2499,#2499,#2164,.T.);
#3002=EDGE_CURVE('',#2499,#2500,#1440,.T.);
#3003=EDGE_CURVE('',#2500,#2500,#2165,.T.);
#3004=EDGE_CURVE('',#2501,#2501,#2166,.T.);
#3005=EDGE_CURVE('',#2501,#2502,#1441,.T.);
#3006=EDGE_CURVE('',#2502,#2502,#2167,.T.);
#3007=EDGE_CURVE('',#2503,#2503,#2168,.T.);
#3008=EDGE_CURVE('',#2503,#2504,#1442,.T.);
#3009=EDGE_CURVE('',#2504,#2504,#2169,.T.);
#3010=EDGE_CURVE('',#2505,#2505,#2170,.T.);
#3011=EDGE_CURVE('',#2506,#2506,#2171,.T.);
#3012=EDGE_CURVE('',#2506,#2505,#1443,.T.);
#3013=EDGE_CURVE('',#2507,#2507,#320,.T.);
#3014=EDGE_CURVE('',#2508,#2508,#2172,.T.);
#3015=EDGE_CURVE('',#2508,#2509,#1444,.T.);
#3016=EDGE_CURVE('',#2509,#2509,#2173,.T.);
#3017=EDGE_CURVE('',#2510,#2510,#2174,.T.);
#3018=EDGE_CURVE('',#2511,#2511,#2175,.T.);
#3019=EDGE_CURVE('',#2511,#2512,#1445,.T.);
#3020=EDGE_CURVE('',#2512,#2512,#2176,.T.);
#3021=EDGE_CURVE('',#2513,#2513,#2177,.T.);
#3022=EDGE_CURVE('',#2514,#2514,#2178,.T.);
#3023=EDGE_CURVE('',#2514,#2515,#1446,.T.);
#3024=EDGE_CURVE('',#2515,#2515,#2179,.T.);
#3025=EDGE_CURVE('',#2516,#2516,#2180,.T.);
#3026=EDGE_CURVE('',#2517,#2517,#2181,.T.);
#3027=EDGE_CURVE('',#2517,#2518,#1447,.T.);
#3028=EDGE_CURVE('',#2518,#2518,#2182,.T.);
#3029=EDGE_CURVE('',#2519,#2519,#2183,.T.);
#3030=EDGE_CURVE('',#2520,#2520,#2184,.T.);
#3031=EDGE_CURVE('',#2520,#2510,#1448,.T.);
#3032=EDGE_CURVE('',#2521,#2521,#2185,.T.);
#3033=EDGE_CURVE('',#2521,#2513,#1449,.T.);
#3034=EDGE_CURVE('',#2522,#2522,#2186,.T.);
#3035=EDGE_CURVE('',#2522,#2516,#1450,.T.);
#3036=EDGE_CURVE('',#2523,#2523,#2187,.T.);
#3037=EDGE_CURVE('',#2523,#2519,#1451,.T.);
#3038=EDGE_CURVE('',#2524,#2524,#2188,.T.);
#3039=EDGE_CURVE('',#2525,#2525,#2189,.T.);
#3040=EDGE_CURVE('',#2526,#2526,#2190,.T.);
#3041=EDGE_CURVE('',#2527,#2527,#2191,.T.);
#3042=EDGE_CURVE('',#2528,#2529,#1452,.T.);
#3043=EDGE_CURVE('',#2529,#2530,#1453,.T.);
#3044=EDGE_CURVE('',#2531,#2530,#1454,.T.);
#3045=EDGE_CURVE('',#2531,#2528,#1455,.T.);
#3046=EDGE_CURVE('',#2530,#2532,#1456,.T.);
#3047=EDGE_CURVE('',#2533,#2529,#1457,.T.);
#3048=EDGE_CURVE('',#2533,#2532,#1458,.T.);
#3049=EDGE_CURVE('',#2532,#2534,#1459,.T.);
#3050=EDGE_CURVE('',#2535,#2533,#1460,.T.);
#3051=EDGE_CURVE('',#2535,#2534,#1461,.T.);
#3052=EDGE_CURVE('',#2536,#2536,#2192,.T.);
#3053=EDGE_CURVE('',#2536,#2494,#1462,.T.);
#3054=EDGE_CURVE('',#2537,#2537,#2193,.T.);
#3055=EDGE_CURVE('',#2537,#2507,#1463,.T.);
#3056=EDGE_CURVE('',#2528,#2535,#1464,.T.);
#3057=EDGE_CURVE('',#2534,#2531,#1465,.T.);
#3058=EDGE_CURVE('',#2538,#2538,#2194,.T.);
#3059=EDGE_CURVE('',#2538,#2539,#1466,.T.);
#3060=EDGE_CURVE('',#2539,#2539,#2195,.T.);
#3061=EDGE_CURVE('',#2540,#2540,#2196,.T.);
#3062=EDGE_CURVE('',#2540,#2541,#1467,.T.);
#3063=EDGE_CURVE('',#2541,#2541,#2197,.T.);
#3064=EDGE_CURVE('',#2542,#2542,#2198,.T.);
#3065=EDGE_CURVE('',#2542,#2543,#1468,.T.);
#3066=EDGE_CURVE('',#2543,#2543,#2199,.T.);
#3067=EDGE_CURVE('',#2544,#2544,#2200,.T.);
#3068=EDGE_CURVE('',#2544,#2545,#1469,.T.);
#3069=EDGE_CURVE('',#2545,#2545,#2201,.T.);
#3070=EDGE_CURVE('',#2546,#2547,#1470,.T.);
#3071=EDGE_CURVE('',#2547,#2548,#1471,.T.);
#3072=EDGE_CURVE('',#2549,#2548,#1472,.T.);
#3073=EDGE_CURVE('',#2546,#2549,#1473,.T.);
#3074=EDGE_CURVE('',#2550,#2546,#1474,.T.);
#3075=EDGE_CURVE('',#2551,#2549,#1475,.T.);
#3076=EDGE_CURVE('',#2550,#2551,#1476,.T.);
#3077=EDGE_CURVE('',#2552,#2550,#1477,.T.);
#3078=EDGE_CURVE('',#2553,#2551,#1478,.T.);
#3079=EDGE_CURVE('',#2552,#2553,#1479,.T.);
#3080=EDGE_CURVE('',#2547,#2552,#1480,.T.);
#3081=EDGE_CURVE('',#2548,#2553,#1481,.T.);
#3082=EDGE_CURVE('',#2554,#2554,#2202,.T.);
#3083=EDGE_CURVE('',#2554,#2527,#1482,.T.);
#3084=EDGE_CURVE('',#2555,#2555,#2203,.T.);
#3085=EDGE_CURVE('',#2555,#2526,#1483,.T.);
#3086=EDGE_CURVE('',#2556,#2556,#2204,.T.);
#3087=EDGE_CURVE('',#2556,#2525,#1484,.T.);
#3088=EDGE_CURVE('',#2557,#2557,#2205,.T.);
#3089=EDGE_CURVE('',#2557,#2524,#1485,.T.);
#3090=EDGE_CURVE('',#2558,#2559,#1486,.T.);
#3091=EDGE_CURVE('',#2559,#2560,#1487,.T.);
#3092=EDGE_CURVE('',#2561,#2560,#1488,.T.);
#3093=EDGE_CURVE('',#2558,#2561,#1489,.T.);
#3094=EDGE_CURVE('',#2562,#2558,#1490,.T.);
#3095=EDGE_CURVE('',#2563,#2561,#1491,.T.);
#3096=EDGE_CURVE('',#2562,#2563,#1492,.T.);
#3097=EDGE_CURVE('',#2564,#2562,#1493,.T.);
#3098=EDGE_CURVE('',#2565,#2563,#1494,.T.);
#3099=EDGE_CURVE('',#2564,#2565,#1495,.T.);
#3100=EDGE_CURVE('',#2559,#2564,#1496,.T.);
#3101=EDGE_CURVE('',#2560,#2565,#1497,.T.);
#3102=EDGE_CURVE('',#2566,#2567,#1498,.T.);
#3103=EDGE_CURVE('',#2567,#2568,#1499,.T.);
#3104=EDGE_CURVE('',#2569,#2568,#1500,.T.);
#3105=EDGE_CURVE('',#2566,#2569,#1501,.T.);
#3106=EDGE_CURVE('',#2570,#2566,#1502,.T.);
#3107=EDGE_CURVE('',#2571,#2569,#1503,.T.);
#3108=EDGE_CURVE('',#2570,#2571,#1504,.T.);
#3109=EDGE_CURVE('',#2572,#2570,#1505,.T.);
#3110=EDGE_CURVE('',#2573,#2571,#1506,.T.);
#3111=EDGE_CURVE('',#2572,#2573,#1507,.T.);
#3112=EDGE_CURVE('',#2567,#2572,#1508,.T.);
#3113=EDGE_CURVE('',#2568,#2573,#1509,.T.);
#3114=EDGE_CURVE('',#2574,#2575,#1510,.T.);
#3115=EDGE_CURVE('',#2576,#2574,#2206,.T.);
#3116=EDGE_CURVE('',#2577,#2576,#1511,.T.);
#3117=EDGE_CURVE('',#2575,#2577,#2207,.T.);
#3118=EDGE_CURVE('',#2576,#2578,#2208,.T.);
#3119=EDGE_CURVE('',#2578,#2574,#2209,.T.);
#3120=EDGE_CURVE('',#2579,#2579,#2210,.T.);
#3121=EDGE_CURVE('',#2580,#2581,#2211,.T.);
#3122=EDGE_CURVE('',#2580,#2581,#2212,.T.);
#3123=EDGE_CURVE('',#2582,#2582,#2213,.T.);
#3124=EDGE_CURVE('',#2583,#2580,#1512,.T.);
#3125=EDGE_CURVE('',#2584,#2583,#2214,.T.);
#3126=EDGE_CURVE('',#2581,#2584,#1513,.T.);
#3127=EDGE_CURVE('',#2585,#2586,#2215,.T.);
#3128=EDGE_CURVE('',#2585,#2586,#2216,.T.);
#3129=EDGE_CURVE('',#2587,#2587,#2217,.T.);
#3130=EDGE_CURVE('',#2588,#2585,#1514,.T.);
#3131=EDGE_CURVE('',#2589,#2588,#2218,.T.);
#3132=EDGE_CURVE('',#2586,#2589,#1515,.T.);
#3133=EDGE_CURVE('',#2590,#2591,#2219,.T.);
#3134=EDGE_CURVE('',#2590,#2591,#2220,.T.);
#3135=EDGE_CURVE('',#2592,#2592,#2221,.T.);
#3136=EDGE_CURVE('',#2593,#2590,#1516,.T.);
#3137=EDGE_CURVE('',#2594,#2593,#2222,.T.);
#3138=EDGE_CURVE('',#2591,#2594,#1517,.T.);
#3139=EDGE_CURVE('',#2577,#2594,#2223,.T.);
#3140=EDGE_CURVE('',#2593,#2589,#2224,.T.);
#3141=EDGE_CURVE('',#2588,#2584,#2225,.T.);
#3142=EDGE_CURVE('',#2583,#2575,#2226,.T.);
#3143=EDGE_CURVE('',#2595,#2595,#2227,.T.);
#3144=EDGE_CURVE('',#2596,#2596,#2228,.T.);
#3145=EDGE_CURVE('',#2596,#2579,#1518,.T.);
#3146=EDGE_CURVE('',#2597,#2597,#2229,.T.);
#3147=EDGE_CURVE('',#2597,#2582,#1519,.T.);
#3148=EDGE_CURVE('',#2598,#2598,#2230,.T.);
#3149=EDGE_CURVE('',#2598,#2587,#1520,.T.);
#3150=EDGE_CURVE('',#2599,#2599,#2231,.T.);
#3151=EDGE_CURVE('',#2599,#2592,#1521,.T.);
#3152=EDGE_CURVE('',#2600,#2600,#2232,.T.);
#3153=EDGE_CURVE('',#2600,#2601,#1522,.T.);
#3154=EDGE_CURVE('',#2601,#2601,#2233,.T.);
#3155=EDGE_CURVE('',#2602,#2602,#2234,.T.);
#3156=EDGE_CURVE('',#2595,#2602,#1523,.T.);
#3157=EDGE_CURVE('',#2578,#2603,#1524,.T.);
#3158=EDGE_CURVE('',#2603,#2603,#2235,.T.);
#3159=EDGE_CURVE('',#2604,#2605,#1525,.T.);
#3160=EDGE_CURVE('',#2606,#2604,#2236,.T.);
#3161=EDGE_CURVE('',#2607,#2606,#1526,.T.);
#3162=EDGE_CURVE('',#2605,#2607,#2237,.T.);
#3163=EDGE_CURVE('',#2606,#2608,#2238,.T.);
#3164=EDGE_CURVE('',#2608,#2604,#2239,.T.);
#3165=EDGE_CURVE('',#2609,#2609,#2240,.T.);
#3166=EDGE_CURVE('',#2610,#2611,#2241,.T.);
#3167=EDGE_CURVE('',#2610,#2611,#2242,.T.);
#3168=EDGE_CURVE('',#2612,#2612,#2243,.T.);
#3169=EDGE_CURVE('',#2613,#2610,#1527,.T.);
#3170=EDGE_CURVE('',#2614,#2613,#2244,.T.);
#3171=EDGE_CURVE('',#2611,#2614,#1528,.T.);
#3172=EDGE_CURVE('',#2615,#2616,#2245,.T.);
#3173=EDGE_CURVE('',#2615,#2616,#2246,.T.);
#3174=EDGE_CURVE('',#2617,#2617,#2247,.T.);
#3175=EDGE_CURVE('',#2618,#2615,#1529,.T.);
#3176=EDGE_CURVE('',#2619,#2618,#2248,.T.);
#3177=EDGE_CURVE('',#2616,#2619,#1530,.T.);
#3178=EDGE_CURVE('',#2620,#2621,#2249,.T.);
#3179=EDGE_CURVE('',#2620,#2621,#2250,.T.);
#3180=EDGE_CURVE('',#2622,#2622,#2251,.T.);
#3181=EDGE_CURVE('',#2623,#2620,#1531,.T.);
#3182=EDGE_CURVE('',#2624,#2623,#2252,.T.);
#3183=EDGE_CURVE('',#2621,#2624,#1532,.T.);
#3184=EDGE_CURVE('',#2607,#2624,#2253,.T.);
#3185=EDGE_CURVE('',#2623,#2619,#2254,.T.);
#3186=EDGE_CURVE('',#2618,#2614,#2255,.T.);
#3187=EDGE_CURVE('',#2613,#2605,#2256,.T.);
#3188=EDGE_CURVE('',#2625,#2625,#2257,.T.);
#3189=EDGE_CURVE('',#2626,#2626,#2258,.T.);
#3190=EDGE_CURVE('',#2626,#2609,#1533,.T.);
#3191=EDGE_CURVE('',#2627,#2627,#2259,.T.);
#3192=EDGE_CURVE('',#2627,#2612,#1534,.T.);
#3193=EDGE_CURVE('',#2628,#2628,#2260,.T.);
#3194=EDGE_CURVE('',#2628,#2617,#1535,.T.);
#3195=EDGE_CURVE('',#2629,#2629,#2261,.T.);
#3196=EDGE_CURVE('',#2629,#2622,#1536,.T.);
#3197=EDGE_CURVE('',#2630,#2630,#2262,.T.);
#3198=EDGE_CURVE('',#2630,#2631,#1537,.T.);
#3199=EDGE_CURVE('',#2631,#2631,#2263,.T.);
#3200=EDGE_CURVE('',#2632,#2632,#2264,.T.);
#3201=EDGE_CURVE('',#2625,#2632,#1538,.T.);
#3202=EDGE_CURVE('',#2608,#2633,#1539,.T.);
#3203=EDGE_CURVE('',#2633,#2633,#2265,.T.);
#3204=EDGE_CURVE('',#2634,#2634,#2266,.T.);
#3205=EDGE_CURVE('',#2635,#2635,#2267,.T.);
#3206=EDGE_CURVE('',#2635,#2634,#1540,.T.);
#3207=EDGE_CURVE('',#2636,#2636,#2268,.T.);
#3208=EDGE_CURVE('',#2636,#2635,#1541,.T.);
#3209=EDGE_CURVE('',#2637,#2637,#2269,.T.);
#3210=EDGE_CURVE('',#2637,#2636,#1542,.T.);
#3211=EDGE_CURVE('',#2638,#2638,#2270,.T.);
#3212=EDGE_CURVE('',#2639,#2639,#2271,.F.);
#3213=EDGE_CURVE('',#2639,#2638,#1543,.T.);
#3214=EDGE_CURVE('',#2640,#2640,#2272,.F.);
#3215=EDGE_CURVE('',#2640,#2639,#1544,.T.);
#3216=EDGE_CURVE('',#2641,#2641,#2273,.T.);
#3217=EDGE_CURVE('',#2641,#2640,#1545,.T.);
#3218=EDGE_CURVE('',#2642,#2643,#1546,.T.);
#3219=EDGE_CURVE('',#2643,#2644,#1547,.T.);
#3220=EDGE_CURVE('',#2644,#2645,#1548,.T.);
#3221=EDGE_CURVE('',#2642,#2645,#1549,.T.);
#3222=EDGE_CURVE('',#2643,#2646,#1550,.T.);
#3223=EDGE_CURVE('',#2646,#2647,#1551,.T.);
#3224=EDGE_CURVE('',#2647,#2644,#1552,.T.);
#3225=EDGE_CURVE('',#2646,#2648,#1553,.T.);
#3226=EDGE_CURVE('',#2648,#2649,#1554,.T.);
#3227=EDGE_CURVE('',#2649,#2647,#1555,.T.);
#3228=EDGE_CURVE('',#2648,#2650,#1556,.T.);
#3229=EDGE_CURVE('',#2650,#2651,#1557,.T.);
#3230=EDGE_CURVE('',#2651,#2649,#1558,.T.);
#3231=EDGE_CURVE('',#2650,#2652,#1559,.T.);
#3232=EDGE_CURVE('',#2652,#2653,#1560,.T.);
#3233=EDGE_CURVE('',#2653,#2651,#1561,.T.);
#3234=EDGE_CURVE('',#2652,#2642,#1562,.T.);
#3235=EDGE_CURVE('',#2645,#2653,#1563,.T.);
#3236=EDGE_CURVE('',#2654,#2655,#2274,.T.);
#3237=EDGE_CURVE('',#2655,#2654,#2275,.T.);
#3238=EDGE_CURVE('',#2655,#2656,#2276,.T.);
#3239=EDGE_CURVE('',#2657,#2656,#2277,.T.);
#3240=EDGE_CURVE('',#2656,#2657,#2278,.T.);
#3241=EDGE_CURVE('',#2657,#2658,#1564,.T.);
#3242=EDGE_CURVE('',#2658,#2658,#2279,.T.);
#3243=EDGE_CURVE('',#2659,#2659,#2280,.T.);
#3244=EDGE_CURVE('',#2659,#2660,#1565,.T.);
#3245=EDGE_CURVE('',#2660,#2660,#2281,.T.);
#3246=EDGE_CURVE('',#2660,#2661,#1566,.T.);
#3247=EDGE_CURVE('',#2661,#2661,#2282,.T.);
#3248=EDGE_CURVE('',#2662,#2662,#2283,.T.);
#3249=EDGE_CURVE('',#2662,#2654,#1567,.T.);
#3250=EDGE_CURVE('',#2663,#2663,#2284,.T.);
#3251=EDGE_CURVE('',#2663,#2659,#1568,.T.);
#3252=EDGE_CURVE('',#2664,#2665,#2285,.T.);
#3253=EDGE_CURVE('',#2665,#2664,#2286,.T.);
#3254=EDGE_CURVE('',#2665,#2666,#2287,.T.);
#3255=EDGE_CURVE('',#2667,#2666,#2288,.T.);
#3256=EDGE_CURVE('',#2666,#2667,#2289,.T.);
#3257=EDGE_CURVE('',#2668,#2668,#2290,.T.);
#3258=EDGE_CURVE('',#2668,#2667,#1569,.T.);
#3259=EDGE_CURVE('',#2669,#2669,#2291,.T.);
#3260=EDGE_CURVE('',#2670,#2670,#2292,.T.);
#3261=EDGE_CURVE('',#2671,#2671,#2293,.T.);
#3262=EDGE_CURVE('',#2671,#2669,#1570,.T.);
#3263=EDGE_CURVE('',#2672,#2672,#2294,.T.);
#3264=EDGE_CURVE('',#2672,#2671,#1571,.T.);
#3265=EDGE_CURVE('',#2673,#2673,#2295,.T.);
#3266=EDGE_CURVE('',#2673,#2672,#1572,.T.);
#3267=EDGE_CURVE('',#2664,#2670,#1573,.T.);
#3268=EDGE_CURVE('',#2674,#2675,#2296,.T.);
#3269=EDGE_CURVE('',#2676,#2677,#2297,.T.);
#3270=EDGE_CURVE('',#2678,#2679,#2298,.T.);
#3271=EDGE_CURVE('',#2680,#2681,#2299,.T.);
#3272=EDGE_CURVE('',#2682,#2683,#2300,.T.);
#3273=EDGE_CURVE('',#2684,#2685,#2301,.T.);
#3274=EDGE_CURVE('',#2686,#2687,#2302,.T.);
#3275=EDGE_CURVE('',#2688,#2689,#2303,.T.);
#3276=EDGE_CURVE('',#2690,#2691,#321,.T.);
#3277=EDGE_CURVE('',#2692,#2690,#2304,.T.);
#3278=EDGE_CURVE('',#2693,#2692,#322,.T.);
#3279=EDGE_CURVE('',#2691,#2693,#2305,.T.);
#3280=EDGE_CURVE('',#2694,#2692,#2306,.T.);
#3281=EDGE_CURVE('',#2694,#2695,#323,.T.);
#3282=EDGE_CURVE('',#2696,#2695,#2307,.T.);
#3283=EDGE_CURVE('',#2696,#2697,#324,.T.);
#3284=EDGE_CURVE('',#2698,#2697,#2308,.T.);
#3285=EDGE_CURVE('',#2698,#2699,#325,.T.);
#3286=EDGE_CURVE('',#2699,#2700,#1574,.T.);
#3287=EDGE_CURVE('',#2700,#2700,#2309,.T.);
#3288=EDGE_CURVE('',#2699,#2701,#326,.T.);
#3289=EDGE_CURVE('',#2702,#2701,#2310,.T.);
#3290=EDGE_CURVE('',#2702,#2703,#327,.T.);
#3291=EDGE_CURVE('',#2704,#2703,#2311,.T.);
#3292=EDGE_CURVE('',#2704,#2705,#328,.T.);
#3293=EDGE_CURVE('',#2706,#2705,#2312,.T.);
#3294=EDGE_CURVE('',#2706,#2707,#329,.T.);
#3295=EDGE_CURVE('',#2708,#2707,#2313,.T.);
#3296=EDGE_CURVE('',#2708,#2709,#330,.T.);
#3297=EDGE_CURVE('',#2693,#2709,#2314,.T.);
#3298=EDGE_CURVE('',#2690,#2710,#2315,.T.);
#3299=EDGE_CURVE('',#2710,#2694,#2316,.T.);
#3300=EDGE_CURVE('',#2711,#2710,#331,.T.);
#3301=EDGE_CURVE('',#2695,#2711,#2317,.T.);
#3302=EDGE_CURVE('',#2711,#2712,#2318,.T.);
#3303=EDGE_CURVE('',#2712,#2696,#2319,.T.);
#3304=EDGE_CURVE('',#2713,#2712,#332,.T.);
#3305=EDGE_CURVE('',#2697,#2713,#2320,.T.);
#3306=EDGE_CURVE('',#2713,#2714,#2321,.T.);
#3307=EDGE_CURVE('',#2714,#2698,#2322,.T.);
#3308=EDGE_CURVE('',#2715,#2716,#333,.T.);
#3309=EDGE_CURVE('',#2701,#2715,#2323,.T.);
#3310=EDGE_CURVE('',#2716,#2714,#334,.T.);
#3311=EDGE_CURVE('',#2715,#2717,#2324,.T.);
#3312=EDGE_CURVE('',#2717,#2702,#2325,.T.);
#3313=EDGE_CURVE('',#2718,#2717,#335,.T.);
#3314=EDGE_CURVE('',#2703,#2718,#2326,.T.);
#3315=EDGE_CURVE('',#2718,#2719,#2327,.T.);
#3316=EDGE_CURVE('',#2719,#2704,#2328,.T.);
#3317=EDGE_CURVE('',#2720,#2719,#336,.T.);
#3318=EDGE_CURVE('',#2705,#2720,#2329,.T.);
#3319=EDGE_CURVE('',#2720,#2721,#2330,.T.);
#3320=EDGE_CURVE('',#2721,#2706,#2331,.T.);
#3321=EDGE_CURVE('',#2722,#2721,#337,.T.);
#3322=EDGE_CURVE('',#2707,#2722,#2332,.T.);
#3323=EDGE_CURVE('',#2723,#2723,#2333,.T.);
#3324=EDGE_CURVE('',#2723,#2716,#1575,.T.);
#3325=EDGE_CURVE('',#2724,#2691,#2334,.T.);
#3326=EDGE_CURVE('',#2724,#2725,#338,.T.);
#3327=EDGE_CURVE('',#2722,#2725,#2335,.T.);
#3328=EDGE_CURVE('',#2709,#2724,#2336,.T.);
#3329=EDGE_CURVE('',#2725,#2708,#2337,.T.);
#3330=EDGE_CURVE('',#2726,#2726,#2338,.T.);
#3331=EDGE_CURVE('',#2727,#2727,#2339,.T.);
#3332=EDGE_CURVE('',#2728,#2728,#2340,.T.);
#3333=EDGE_CURVE('',#2728,#2726,#1576,.T.);
#3334=EDGE_CURVE('',#2729,#2729,#2341,.T.);
#3335=EDGE_CURVE('',#2729,#2727,#1577,.T.);
#3336=EDGE_CURVE('',#2730,#2730,#2342,.T.);
#3337=EDGE_CURVE('',#2731,#2731,#2343,.T.);
#3338=EDGE_CURVE('',#2732,#2732,#2344,.T.);
#3339=EDGE_CURVE('',#2732,#2730,#1578,.T.);
#3340=EDGE_CURVE('',#2733,#2733,#2345,.T.);
#3341=EDGE_CURVE('',#2733,#2731,#1579,.T.);
#3342=EDGE_CURVE('',#2734,#2734,#2346,.T.);
#3343=EDGE_CURVE('',#2734,#2735,#1580,.T.);
#3344=EDGE_CURVE('',#2735,#2735,#2347,.T.);
#3345=EDGE_CURVE('',#2736,#2736,#2348,.T.);
#3346=EDGE_CURVE('',#2736,#2737,#1581,.T.);
#3347=EDGE_CURVE('',#2737,#2737,#2349,.T.);
#3348=EDGE_CURVE('',#2738,#2739,#1582,.T.);
#3349=EDGE_CURVE('',#2740,#2739,#2350,.T.);
#3350=EDGE_CURVE('',#2741,#2740,#1583,.T.);
#3351=EDGE_CURVE('',#2741,#2738,#2351,.T.);
#3352=EDGE_CURVE('',#2742,#2741,#1584,.T.);
#3353=EDGE_CURVE('',#2743,#2742,#2352,.T.);
#3354=EDGE_CURVE('',#2744,#2743,#1585,.T.);
#3355=EDGE_CURVE('',#2745,#2744,#1586,.T.);
#3356=EDGE_CURVE('',#2746,#2745,#1587,.T.);
#3357=EDGE_CURVE('',#2747,#2746,#2353,.T.);
#3358=EDGE_CURVE('',#2738,#2747,#1588,.T.);
#3359=EDGE_CURVE('',#2748,#2748,#2354,.T.);
#3360=EDGE_CURVE('',#2749,#2747,#1589,.T.);
#3361=EDGE_CURVE('',#2739,#2749,#1590,.T.);
#3362=EDGE_CURVE('',#2742,#2750,#1591,.T.);
#3363=EDGE_CURVE('',#2750,#2740,#1592,.T.);
#3364=EDGE_CURVE('',#2751,#2743,#1593,.T.);
#3365=EDGE_CURVE('',#2752,#2751,#1594,.T.);
#3366=EDGE_CURVE('',#2744,#2752,#1595,.T.);
#3367=EDGE_CURVE('',#2746,#2753,#1596,.T.);
#3368=EDGE_CURVE('',#2745,#2754,#1597,.T.);
#3369=EDGE_CURVE('',#2753,#2754,#1598,.T.);
#3370=EDGE_CURVE('',#2754,#2752,#1599,.T.);
#3371=EDGE_CURVE('',#2749,#2753,#2355,.T.);
#3372=EDGE_CURVE('',#2751,#2750,#2356,.T.);
#3373=EDGE_CURVE('',#2755,#2755,#2357,.T.);
#3374=EDGE_CURVE('',#2756,#2756,#2358,.T.);
#3375=EDGE_CURVE('',#2757,#2757,#2359,.T.);
#3376=EDGE_CURVE('',#2748,#2756,#1600,.T.);
#3377=EDGE_CURVE('',#2757,#2758,#1601,.T.);
#3378=EDGE_CURVE('',#2758,#2758,#2360,.T.);
#3379=EDGE_CURVE('',#2759,#2759,#2361,.T.);
#3380=EDGE_CURVE('',#2759,#2755,#1602,.T.);
#3381=EDGE_CURVE('',#2760,#2760,#2362,.T.);
#3382=EDGE_CURVE('',#2760,#2761,#1603,.T.);
#3383=EDGE_CURVE('',#2761,#2761,#2363,.T.);
#3384=EDGE_CURVE('',#2762,#2762,#2364,.T.);
#3385=EDGE_CURVE('',#2762,#2763,#1604,.T.);
#3386=EDGE_CURVE('',#2763,#2763,#2365,.T.);
#3387=EDGE_CURVE('',#2764,#2765,#1605,.T.);
#3388=EDGE_CURVE('',#2766,#2764,#2366,.T.);
#3389=EDGE_CURVE('',#2765,#2766,#2367,.T.);
#3390=EDGE_CURVE('',#2767,#2767,#339,.T.);
#3391=EDGE_CURVE('',#2767,#2766,#1606,.T.);
#3392=EDGE_CURVE('',#2768,#2764,#340,.T.);
#3393=EDGE_CURVE('',#2768,#2769,#2368,.T.);
#3394=EDGE_CURVE('',#2765,#2769,#341,.T.);
#3395=EDGE_CURVE('',#2769,#2768,#1607,.T.);
#3396=EDGE_CURVE('',#2770,#2771,#1608,.T.);
#3397=EDGE_CURVE('',#2771,#2770,#2369,.T.);
#3398=EDGE_CURVE('',#2772,#2773,#342,.T.);
#3399=EDGE_CURVE('',#2774,#2772,#343,.T.);
#3400=EDGE_CURVE('',#2773,#2774,#344,.T.);
#3401=EDGE_CURVE('',#2773,#2775,#1609,.T.);
#3402=EDGE_CURVE('',#2776,#2775,#345,.T.);
#3403=EDGE_CURVE('',#2776,#2777,#2370,.T.);
#3404=EDGE_CURVE('',#2778,#2777,#346,.T.);
#3405=EDGE_CURVE('',#2771,#2778,#347,.T.);
#3406=EDGE_CURVE('',#2775,#2770,#348,.T.);
#3407=EDGE_CURVE('',#2777,#2776,#1610,.T.);
#3408=EDGE_CURVE('',#2779,#2779,#2371,.T.);
#3409=EDGE_CURVE('',#2779,#2775,#1611,.T.);
#3410=EDGE_CURVE('',#2778,#2780,#1612,.T.);
#3411=EDGE_CURVE('',#2780,#2780,#2372,.T.);
#3412=EDGE_CURVE('',#2781,#2781,#2373,.T.);
#3413=EDGE_CURVE('',#2781,#2773,#1613,.T.);
#3414=EDGE_CURVE('',#2774,#2782,#1614,.T.);
#3415=EDGE_CURVE('',#2782,#2782,#2374,.T.);
#3416=EDGE_CURVE('',#2783,#2783,#2375,.T.);
#3417=EDGE_CURVE('',#2784,#2784,#2376,.T.);
#3418=EDGE_CURVE('',#2785,#2785,#2377,.T.);
#3419=EDGE_CURVE('',#2786,#2786,#2378,.T.);
#3420=EDGE_CURVE('',#2783,#2785,#1615,.T.);
#3421=EDGE_CURVE('',#2786,#2787,#1616,.T.);
#3422=EDGE_CURVE('',#2787,#2787,#2379,.T.);
#3423=EDGE_CURVE('',#2788,#2788,#2380,.T.);
#3424=EDGE_CURVE('',#2788,#2784,#1617,.T.);
#3425=EDGE_CURVE('',#2789,#2789,#2381,.T.);
#3426=EDGE_CURVE('',#2789,#2790,#1618,.T.);
#3427=EDGE_CURVE('',#2790,#2790,#2382,.T.);
#3428=EDGE_CURVE('',#2791,#2792,#1619,.T.);
#3429=EDGE_CURVE('',#2793,#2791,#2383,.T.);
#3430=EDGE_CURVE('',#2794,#2793,#1620,.T.);
#3431=EDGE_CURVE('',#2794,#2792,#2384,.T.);
#3432=EDGE_CURVE('',#2794,#2795,#1621,.T.);
#3433=EDGE_CURVE('',#2796,#2795,#2385,.T.);
#3434=EDGE_CURVE('',#2796,#2792,#1622,.T.);
#3435=EDGE_CURVE('',#2797,#2793,#1623,.T.);
#3436=EDGE_CURVE('',#2795,#2797,#1624,.T.);
#3437=EDGE_CURVE('',#2798,#2796,#1625,.T.);
#3438=EDGE_CURVE('',#2791,#2798,#1626,.T.);
#3439=EDGE_CURVE('',#2798,#2797,#2386,.T.);
#3440=EDGE_CURVE('',#2799,#2799,#2387,.T.);
#3441=EDGE_CURVE('',#2799,#2800,#1627,.T.);
#3442=EDGE_CURVE('',#2800,#2800,#2388,.T.);
#3443=EDGE_CURVE('',#2801,#2801,#2389,.T.);
#3444=EDGE_CURVE('',#2801,#2802,#1628,.T.);
#3445=EDGE_CURVE('',#2802,#2802,#2390,.T.);
#3446=EDGE_CURVE('',#2803,#2803,#2391,.T.);
#3447=EDGE_CURVE('',#2803,#2804,#1629,.T.);
#3448=EDGE_CURVE('',#2804,#2804,#2392,.T.);
#3449=EDGE_CURVE('',#2805,#2805,#2393,.T.);
#3450=EDGE_CURVE('',#2805,#2806,#1630,.T.);
#3451=EDGE_CURVE('',#2806,#2806,#2394,.T.);
#3452=EDGE_CURVE('',#2807,#2807,#2395,.T.);
#3453=EDGE_CURVE('',#2807,#2808,#1631,.T.);
#3454=EDGE_CURVE('',#2808,#2808,#2396,.T.);
#3455=EDGE_CURVE('',#2809,#2809,#2397,.T.);
#3456=EDGE_CURVE('',#2809,#2810,#1632,.T.);
#3457=EDGE_CURVE('',#2810,#2810,#2398,.T.);
#3458=EDGE_CURVE('',#2811,#2812,#1633,.T.);
#3459=EDGE_CURVE('',#2812,#2813,#1634,.T.);
#3460=EDGE_CURVE('',#2813,#2814,#1635,.T.);
#3461=EDGE_CURVE('',#2811,#2814,#1636,.T.);
#3462=EDGE_CURVE('',#2812,#2815,#1637,.T.);
#3463=EDGE_CURVE('',#2815,#2816,#1638,.T.);
#3464=EDGE_CURVE('',#2816,#2813,#1639,.T.);
#3465=EDGE_CURVE('',#2815,#2817,#1640,.T.);
#3466=EDGE_CURVE('',#2817,#2818,#1641,.T.);
#3467=EDGE_CURVE('',#2818,#2816,#1642,.T.);
#3468=EDGE_CURVE('',#2817,#2819,#1643,.T.);
#3469=EDGE_CURVE('',#2819,#2820,#1644,.T.);
#3470=EDGE_CURVE('',#2820,#2818,#1645,.T.);
#3471=EDGE_CURVE('',#2819,#2821,#1646,.T.);
#3472=EDGE_CURVE('',#2821,#2822,#1647,.T.);
#3473=EDGE_CURVE('',#2822,#2820,#1648,.T.);
#3474=EDGE_CURVE('',#2821,#2811,#1649,.T.);
#3475=EDGE_CURVE('',#2814,#2822,#1650,.T.);
#3476=EDGE_CURVE('',#2823,#2823,#2399,.T.);
#3477=EDGE_CURVE('',#2824,#2824,#2400,.T.);
#3478=EDGE_CURVE('',#2825,#2825,#2401,.T.);
#3479=EDGE_CURVE('',#2825,#2824,#1651,.T.);
#3480=EDGE_CURVE('',#2826,#2826,#2402,.T.);
#3481=EDGE_CURVE('',#2826,#2825,#1652,.T.);
#3482=EDGE_CURVE('',#2827,#2827,#2403,.T.);
#3483=EDGE_CURVE('',#2827,#2826,#1653,.T.);
#3484=EDGE_CURVE('',#2828,#2828,#2404,.T.);
#3485=EDGE_CURVE('',#2829,#2829,#2405,.F.);
#3486=EDGE_CURVE('',#2829,#2828,#1654,.T.);
#3487=EDGE_CURVE('',#2823,#2829,#1655,.T.);
#3488=EDGE_CURVE('',#2830,#2830,#2406,.T.);
#3489=EDGE_CURVE('',#2830,#2831,#1656,.T.);
#3490=EDGE_CURVE('',#2831,#2831,#2407,.T.);
#3491=EDGE_CURVE('',#2832,#2832,#2408,.T.);
#3492=EDGE_CURVE('',#2832,#2833,#1657,.T.);
#3493=EDGE_CURVE('',#2833,#2833,#2409,.T.);
#3494=EDGE_CURVE('',#2834,#2834,#2410,.T.);
#3495=EDGE_CURVE('',#2834,#2835,#1658,.T.);
#3496=EDGE_CURVE('',#2835,#2835,#2411,.T.);
#3497=EDGE_CURVE('',#2836,#2836,#2412,.T.);
#3498=EDGE_CURVE('',#2836,#2837,#1659,.T.);
#3499=EDGE_CURVE('',#2837,#2837,#2413,.T.);
#3500=EDGE_CURVE('',#2838,#2839,#2414,.T.);
#3501=EDGE_CURVE('',#2840,#2838,#1660,.T.);
#3502=EDGE_CURVE('',#2841,#2840,#2415,.T.);
#3503=EDGE_CURVE('',#2839,#2841,#1661,.T.);
#3504=EDGE_CURVE('',#2842,#2843,#2416,.T.);
#3505=EDGE_CURVE('',#2844,#2842,#1662,.T.);
#3506=EDGE_CURVE('',#2845,#2844,#2417,.T.);
#3507=EDGE_CURVE('',#2843,#2845,#1663,.T.);
#3508=EDGE_CURVE('',#2846,#2847,#2418,.T.);
#3509=EDGE_CURVE('',#2848,#2846,#1664,.T.);
#3510=EDGE_CURVE('',#2849,#2848,#2419,.T.);
#3511=EDGE_CURVE('',#2847,#2849,#1665,.T.);
#3512=EDGE_CURVE('',#2850,#2851,#1666,.T.);
#3513=EDGE_CURVE('',#2852,#2850,#2420,.T.);
#3514=EDGE_CURVE('',#2853,#2852,#1667,.T.);
#3515=EDGE_CURVE('',#2851,#2853,#2421,.T.);
#3516=EDGE_CURVE('',#2838,#2854,#2422,.T.);
#3517=EDGE_CURVE('',#2854,#2855,#1668,.T.);
#3518=EDGE_CURVE('',#2840,#2855,#2423,.T.);
#3519=EDGE_CURVE('',#2842,#2856,#2424,.T.);
#3520=EDGE_CURVE('',#2856,#2857,#1669,.T.);
#3521=EDGE_CURVE('',#2844,#2857,#2425,.T.);
#3522=EDGE_CURVE('',#2846,#2858,#2426,.T.);
#3523=EDGE_CURVE('',#2858,#2859,#1670,.T.);
#3524=EDGE_CURVE('',#2848,#2859,#2427,.T.);
#3525=EDGE_CURVE('',#2855,#2860,#1671,.T.);
#3526=EDGE_CURVE('',#2860,#2861,#1672,.T.);
#3527=EDGE_CURVE('',#2861,#2862,#1673,.T.);
#3528=EDGE_CURVE('',#2862,#2863,#2428,.T.);
#3529=EDGE_CURVE('',#2863,#2864,#1674,.T.);
#3530=EDGE_CURVE('',#2864,#2865,#1675,.T.);
#3531=EDGE_CURVE('',#2865,#2866,#1676,.T.);
#3532=EDGE_CURVE('',#2866,#2852,#2429,.T.);
#3533=EDGE_CURVE('',#2850,#2867,#2430,.T.);
#3534=EDGE_CURVE('',#2867,#2868,#1677,.T.);
#3535=EDGE_CURVE('',#2868,#2869,#1678,.T.);
#3536=EDGE_CURVE('',#2869,#2870,#1679,.T.);
#3537=EDGE_CURVE('',#2870,#2871,#2431,.T.);
#3538=EDGE_CURVE('',#2871,#2872,#1680,.T.);
#3539=EDGE_CURVE('',#2872,#2873,#1681,.T.);
#3540=EDGE_CURVE('',#2873,#2874,#1682,.T.);
#3541=EDGE_CURVE('',#2874,#2849,#2432,.T.);
#3542=EDGE_CURVE('',#2859,#2875,#1683,.T.);
#3543=EDGE_CURVE('',#2875,#2876,#1684,.T.);
#3544=EDGE_CURVE('',#2876,#2877,#1685,.T.);
#3545=EDGE_CURVE('',#2877,#2878,#2433,.T.);
#3546=EDGE_CURVE('',#2878,#2879,#1686,.T.);
#3547=EDGE_CURVE('',#2879,#2880,#1687,.T.);
#3548=EDGE_CURVE('',#2880,#2881,#1688,.T.);
#3549=EDGE_CURVE('',#2881,#2845,#2434,.T.);
#3550=EDGE_CURVE('',#2857,#2882,#1689,.T.);
#3551=EDGE_CURVE('',#2882,#2883,#1690,.T.);
#3552=EDGE_CURVE('',#2883,#2884,#1691,.T.);
#3553=EDGE_CURVE('',#2884,#2885,#2435,.T.);
#3554=EDGE_CURVE('',#2885,#2886,#1692,.T.);
#3555=EDGE_CURVE('',#2886,#2887,#1693,.T.);
#3556=EDGE_CURVE('',#2887,#2888,#1694,.T.);
#3557=EDGE_CURVE('',#2888,#2841,#2436,.T.);
#3558=EDGE_CURVE('',#2851,#2889,#2437,.T.);
#3559=EDGE_CURVE('',#2889,#2867,#1695,.T.);
#3560=EDGE_CURVE('',#2866,#2890,#1696,.T.);
#3561=EDGE_CURVE('',#2890,#2853,#2438,.T.);
#3562=EDGE_CURVE('',#2891,#2865,#1697,.T.);
#3563=EDGE_CURVE('',#2890,#2891,#1698,.T.);
#3564=EDGE_CURVE('',#2892,#2864,#1699,.T.);
#3565=EDGE_CURVE('',#2891,#2892,#1700,.T.);
#3566=EDGE_CURVE('',#2893,#2860,#1701,.T.);
#3567=EDGE_CURVE('',#2894,#2893,#1702,.T.);
#3568=EDGE_CURVE('',#2861,#2894,#1703,.T.);
#3569=EDGE_CURVE('',#2893,#2854,#1704,.T.);
#3570=EDGE_CURVE('',#2895,#2894,#1705,.T.);
#3571=EDGE_CURVE('',#2895,#2862,#1706,.T.);
#3572=EDGE_CURVE('',#2896,#2839,#2439,.T.);
#3573=EDGE_CURVE('',#2896,#2897,#1707,.T.);
#3574=EDGE_CURVE('',#2897,#2898,#1708,.T.);
#3575=EDGE_CURVE('',#2898,#2899,#1709,.T.);
#3576=EDGE_CURVE('',#2899,#2900,#2440,.T.);
#3577=EDGE_CURVE('',#2900,#2901,#2441,.T.);
#3578=EDGE_CURVE('',#2901,#2895,#2442,.T.);
#3579=EDGE_CURVE('',#2892,#2902,#1710,.T.);
#3580=EDGE_CURVE('',#2902,#2903,#2443,.T.);
#3581=EDGE_CURVE('',#2903,#2904,#2444,.T.);
#3582=EDGE_CURVE('',#2904,#2905,#2445,.T.);
#3583=EDGE_CURVE('',#2905,#2906,#1711,.T.);
#3584=EDGE_CURVE('',#2906,#2907,#1712,.T.);
#3585=EDGE_CURVE('',#2907,#2889,#1713,.T.);
#3586=EDGE_CURVE('',#2908,#2909,#2446,.T.);
#3587=EDGE_CURVE('',#2908,#2909,#2447,.T.);
#3588=EDGE_CURVE('',#2903,#2908,#1714,.T.);
#3589=EDGE_CURVE('',#2902,#2863,#1715,.T.);
#3590=EDGE_CURVE('',#2909,#2901,#1716,.T.);
#3591=EDGE_CURVE('',#2900,#2910,#1717,.T.);
#3592=EDGE_CURVE('',#2910,#2911,#2448,.T.);
#3593=EDGE_CURVE('',#2911,#2912,#1718,.T.);
#3594=EDGE_CURVE('',#2912,#2912,#2449,.T.);
#3595=EDGE_CURVE('',#2911,#2913,#2450,.T.);
#3596=EDGE_CURVE('',#2913,#2914,#1719,.T.);
#3597=EDGE_CURVE('',#2915,#2914,#2451,.T.);
#3598=EDGE_CURVE('',#2915,#2916,#1720,.T.);
#3599=EDGE_CURVE('',#2916,#2917,#2452,.T.);
#3600=EDGE_CURVE('',#2917,#2918,#1721,.T.);
#3601=EDGE_CURVE('',#2919,#2918,#2453,.T.);
#3602=EDGE_CURVE('',#2919,#2920,#1722,.T.);
#3603=EDGE_CURVE('',#2920,#2921,#2454,.T.);
#3604=EDGE_CURVE('',#2921,#2904,#1723,.T.);
#3605=EDGE_CURVE('',#2888,#2896,#1724,.T.);
#3606=EDGE_CURVE('',#2897,#2887,#1725,.T.);
#3607=EDGE_CURVE('',#2898,#2886,#1726,.T.);
#3608=EDGE_CURVE('',#2922,#2882,#1727,.T.);
#3609=EDGE_CURVE('',#2923,#2922,#1728,.T.);
#3610=EDGE_CURVE('',#2883,#2923,#1729,.T.);
#3611=EDGE_CURVE('',#2922,#2856,#1730,.T.);
#3612=EDGE_CURVE('',#2924,#2923,#1731,.T.);
#3613=EDGE_CURVE('',#2924,#2884,#1732,.T.);
#3614=EDGE_CURVE('',#2925,#2843,#2455,.T.);
#3615=EDGE_CURVE('',#2925,#2926,#1733,.T.);
#3616=EDGE_CURVE('',#2926,#2927,#1734,.T.);
#3617=EDGE_CURVE('',#2927,#2928,#1735,.T.);
#3618=EDGE_CURVE('',#2928,#2915,#2456,.T.);
#3619=EDGE_CURVE('',#2914,#2924,#2457,.T.);
#3620=EDGE_CURVE('',#2910,#2913,#2458,.T.);
#3621=EDGE_CURVE('',#2899,#2885,#1736,.T.);
#3622=EDGE_CURVE('',#2881,#2925,#1737,.T.);
#3623=EDGE_CURVE('',#2926,#2880,#1738,.T.);
#3624=EDGE_CURVE('',#2927,#2879,#1739,.T.);
#3625=EDGE_CURVE('',#2929,#2875,#1740,.T.);
#3626=EDGE_CURVE('',#2930,#2929,#1741,.T.);
#3627=EDGE_CURVE('',#2876,#2930,#1742,.T.);
#3628=EDGE_CURVE('',#2929,#2858,#1743,.T.);
#3629=EDGE_CURVE('',#2931,#2930,#1744,.T.);
#3630=EDGE_CURVE('',#2931,#2877,#1745,.T.);
#3631=EDGE_CURVE('',#2932,#2847,#2459,.T.);
#3632=EDGE_CURVE('',#2932,#2933,#1746,.T.);
#3633=EDGE_CURVE('',#2933,#2934,#1747,.T.);
#3634=EDGE_CURVE('',#2934,#2935,#1748,.T.);
#3635=EDGE_CURVE('',#2935,#2919,#2460,.T.);
#3636=EDGE_CURVE('',#2918,#2931,#2461,.T.);
#3637=EDGE_CURVE('',#2916,#2917,#2462,.T.);
#3638=EDGE_CURVE('',#2928,#2878,#1749,.T.);
#3639=EDGE_CURVE('',#2874,#2932,#1750,.T.);
#3640=EDGE_CURVE('',#2933,#2873,#1751,.T.);
#3641=EDGE_CURVE('',#2907,#2868,#1752,.T.);
#3642=EDGE_CURVE('',#2869,#2906,#1753,.T.);
#3643=EDGE_CURVE('',#2934,#2872,#1754,.T.);
#3644=EDGE_CURVE('',#2920,#2921,#2463,.T.);
#3645=EDGE_CURVE('',#2935,#2871,#1755,.T.);
#3646=EDGE_CURVE('',#2905,#2870,#1756,.T.);
#3647=EDGE_CURVE('',#2936,#2936,#2464,.T.);
#3648=EDGE_CURVE('',#2936,#2937,#1757,.T.);
#3649=EDGE_CURVE('',#2937,#2937,#2465,.T.);
#3650=EDGE_CURVE('',#2938,#2938,#2466,.T.);
#3651=EDGE_CURVE('',#2938,#2939,#1758,.T.);
#3652=EDGE_CURVE('',#2939,#2939,#2467,.T.);
#3653=EDGE_CURVE('',#2940,#2940,#2468,.T.);
#3654=EDGE_CURVE('',#2940,#2941,#1759,.T.);
#3655=EDGE_CURVE('',#2941,#2941,#2469,.T.);
#3656=EDGE_CURVE('',#2942,#2943,#1760,.T.);
#3657=EDGE_CURVE('',#2944,#2942,#2470,.T.);
#3658=EDGE_CURVE('',#2943,#2944,#2471,.T.);
#3659=EDGE_CURVE('',#2945,#2945,#349,.T.);
#3660=EDGE_CURVE('',#2945,#2944,#1761,.T.);
#3661=EDGE_CURVE('',#2946,#2942,#350,.T.);
#3662=EDGE_CURVE('',#2946,#2947,#2472,.T.);
#3663=EDGE_CURVE('',#2943,#2947,#351,.T.);
#3664=EDGE_CURVE('',#2947,#2946,#1762,.T.);
#3665=EDGE_CURVE('',#2948,#2949,#1763,.T.);
#3666=EDGE_CURVE('',#2949,#2948,#2473,.T.);
#3667=EDGE_CURVE('',#2950,#2951,#352,.T.);
#3668=EDGE_CURVE('',#2952,#2950,#353,.T.);
#3669=EDGE_CURVE('',#2951,#2952,#354,.T.);
#3670=EDGE_CURVE('',#2951,#2953,#1764,.T.);
#3671=EDGE_CURVE('',#2954,#2953,#355,.T.);
#3672=EDGE_CURVE('',#2954,#2955,#2474,.T.);
#3673=EDGE_CURVE('',#2956,#2955,#356,.T.);
#3674=EDGE_CURVE('',#2949,#2956,#357,.T.);
#3675=EDGE_CURVE('',#2953,#2948,#358,.T.);
#3676=EDGE_CURVE('',#2955,#2954,#1765,.T.);
#3677=EDGE_CURVE('',#2957,#2957,#2475,.T.);
#3678=EDGE_CURVE('',#2957,#2953,#1766,.T.);
#3679=EDGE_CURVE('',#2956,#2958,#1767,.T.);
#3680=EDGE_CURVE('',#2958,#2958,#2476,.T.);
#3681=EDGE_CURVE('',#2959,#2959,#2477,.T.);
#3682=EDGE_CURVE('',#2959,#2951,#1768,.T.);
#3683=EDGE_CURVE('',#2952,#2960,#1769,.T.);
#3684=EDGE_CURVE('',#2960,#2960,#2478,.T.);
#3685=EDGE_CURVE('',#2961,#2961,#2479,.T.);
#3686=EDGE_CURVE('',#2962,#2963,#1770,.T.);
#3687=EDGE_CURVE('',#2962,#2964,#1771,.T.);
#3688=EDGE_CURVE('',#2964,#2965,#1772,.T.);
#3689=EDGE_CURVE('',#2963,#2965,#1773,.T.);
#3690=EDGE_CURVE('',#2966,#2962,#1774,.T.);
#3691=EDGE_CURVE('',#2966,#2967,#1775,.T.);
#3692=EDGE_CURVE('',#2967,#2964,#1776,.T.);
#3693=EDGE_CURVE('',#2968,#2966,#1777,.T.);
#3694=EDGE_CURVE('',#2968,#2969,#1778,.T.);
#3695=EDGE_CURVE('',#2969,#2967,#1779,.T.);
#3696=EDGE_CURVE('',#2970,#2968,#1780,.T.);
#3697=EDGE_CURVE('',#2970,#2971,#1781,.T.);
#3698=EDGE_CURVE('',#2971,#2969,#1782,.T.);
#3699=EDGE_CURVE('',#2972,#2970,#1783,.T.);
#3700=EDGE_CURVE('',#2972,#2973,#1784,.T.);
#3701=EDGE_CURVE('',#2973,#2971,#1785,.T.);
#3702=EDGE_CURVE('',#2963,#2972,#1786,.T.);
#3703=EDGE_CURVE('',#2965,#2973,#1787,.T.);
#3704=EDGE_CURVE('',#2974,#2974,#2480,.T.);
#3705=EDGE_CURVE('',#2975,#2975,#2481,.T.);
#3706=EDGE_CURVE('',#2975,#2974,#1788,.T.);
#3707=EDGE_CURVE('',#2961,#2975,#1789,.T.);
#3708=ORIENTED_EDGE('',*,*,#2976,.F.);
#3709=ORIENTED_EDGE('',*,*,#2977,.T.);
#3710=ORIENTED_EDGE('',*,*,#2978,.F.);
#3711=ORIENTED_EDGE('',*,*,#2977,.F.);
#3712=ORIENTED_EDGE('',*,*,#2976,.T.);
#3713=ORIENTED_EDGE('',*,*,#2979,.F.);
#3714=ORIENTED_EDGE('',*,*,#2980,.T.);
#3715=ORIENTED_EDGE('',*,*,#2981,.F.);
#3716=ORIENTED_EDGE('',*,*,#2980,.F.);
#3717=ORIENTED_EDGE('',*,*,#2979,.T.);
#3718=ORIENTED_EDGE('',*,*,#2982,.F.);
#3719=ORIENTED_EDGE('',*,*,#2983,.T.);
#3720=ORIENTED_EDGE('',*,*,#2984,.F.);
#3721=ORIENTED_EDGE('',*,*,#2983,.F.);
#3722=ORIENTED_EDGE('',*,*,#2982,.T.);
#3723=ORIENTED_EDGE('',*,*,#2985,.F.);
#3724=ORIENTED_EDGE('',*,*,#2986,.T.);
#3725=ORIENTED_EDGE('',*,*,#2987,.F.);
#3726=ORIENTED_EDGE('',*,*,#2986,.F.);
#3727=ORIENTED_EDGE('',*,*,#2985,.T.);
#3728=ORIENTED_EDGE('',*,*,#2988,.F.);
#3729=ORIENTED_EDGE('',*,*,#2989,.T.);
#3730=ORIENTED_EDGE('',*,*,#2990,.F.);
#3731=ORIENTED_EDGE('',*,*,#2989,.F.);
#3732=ORIENTED_EDGE('',*,*,#2988,.T.);
#3733=ORIENTED_EDGE('',*,*,#2991,.F.);
#3734=ORIENTED_EDGE('',*,*,#2992,.F.);
#3735=ORIENTED_EDGE('',*,*,#2993,.T.);
#3736=ORIENTED_EDGE('',*,*,#2991,.T.);
#3737=ORIENTED_EDGE('',*,*,#2993,.F.);
#3738=ORIENTED_EDGE('',*,*,#2994,.T.);
#3739=ORIENTED_EDGE('',*,*,#2995,.F.);
#3740=ORIENTED_EDGE('',*,*,#2996,.T.);
#3741=ORIENTED_EDGE('',*,*,#2997,.F.);
#3742=ORIENTED_EDGE('',*,*,#2996,.F.);
#3743=ORIENTED_EDGE('',*,*,#2995,.T.);
#3744=ORIENTED_EDGE('',*,*,#2998,.F.);
#3745=ORIENTED_EDGE('',*,*,#2999,.T.);
#3746=ORIENTED_EDGE('',*,*,#3000,.F.);
#3747=ORIENTED_EDGE('',*,*,#2999,.F.);
#3748=ORIENTED_EDGE('',*,*,#2998,.T.);
#3749=ORIENTED_EDGE('',*,*,#3001,.F.);
#3750=ORIENTED_EDGE('',*,*,#3002,.T.);
#3751=ORIENTED_EDGE('',*,*,#3003,.F.);
#3752=ORIENTED_EDGE('',*,*,#3002,.F.);
#3753=ORIENTED_EDGE('',*,*,#3001,.T.);
#3754=ORIENTED_EDGE('',*,*,#3004,.F.);
#3755=ORIENTED_EDGE('',*,*,#3005,.T.);
#3756=ORIENTED_EDGE('',*,*,#3006,.F.);
#3757=ORIENTED_EDGE('',*,*,#3005,.F.);
#3758=ORIENTED_EDGE('',*,*,#3004,.T.);
#3759=ORIENTED_EDGE('',*,*,#3007,.F.);
#3760=ORIENTED_EDGE('',*,*,#3008,.T.);
#3761=ORIENTED_EDGE('',*,*,#3009,.F.);
#3762=ORIENTED_EDGE('',*,*,#3008,.F.);
#3763=ORIENTED_EDGE('',*,*,#3007,.T.);
#3764=ORIENTED_EDGE('',*,*,#3010,.F.);
#3765=ORIENTED_EDGE('',*,*,#3011,.F.);
#3766=ORIENTED_EDGE('',*,*,#3012,.T.);
#3767=ORIENTED_EDGE('',*,*,#3010,.T.);
#3768=ORIENTED_EDGE('',*,*,#3012,.F.);
#3769=ORIENTED_EDGE('',*,*,#3013,.T.);
#3770=ORIENTED_EDGE('',*,*,#3014,.F.);
#3771=ORIENTED_EDGE('',*,*,#3015,.T.);
#3772=ORIENTED_EDGE('',*,*,#3016,.F.);
#3773=ORIENTED_EDGE('',*,*,#3015,.F.);
#3774=ORIENTED_EDGE('',*,*,#3014,.T.);
#3775=ORIENTED_EDGE('',*,*,#3017,.F.);
#3776=ORIENTED_EDGE('',*,*,#3018,.F.);
#3777=ORIENTED_EDGE('',*,*,#3019,.T.);
#3778=ORIENTED_EDGE('',*,*,#3020,.F.);
#3779=ORIENTED_EDGE('',*,*,#3019,.F.);
#3780=ORIENTED_EDGE('',*,*,#3018,.T.);
#3781=ORIENTED_EDGE('',*,*,#3021,.F.);
#3782=ORIENTED_EDGE('',*,*,#3022,.F.);
#3783=ORIENTED_EDGE('',*,*,#3023,.T.);
#3784=ORIENTED_EDGE('',*,*,#3024,.F.);
#3785=ORIENTED_EDGE('',*,*,#3023,.F.);
#3786=ORIENTED_EDGE('',*,*,#3022,.T.);
#3787=ORIENTED_EDGE('',*,*,#3025,.F.);
#3788=ORIENTED_EDGE('',*,*,#3026,.F.);
#3789=ORIENTED_EDGE('',*,*,#3027,.T.);
#3790=ORIENTED_EDGE('',*,*,#3028,.F.);
#3791=ORIENTED_EDGE('',*,*,#3027,.F.);
#3792=ORIENTED_EDGE('',*,*,#3026,.T.);
#3793=ORIENTED_EDGE('',*,*,#3029,.F.);
#3794=ORIENTED_EDGE('',*,*,#3030,.F.);
#3795=ORIENTED_EDGE('',*,*,#3031,.T.);
#3796=ORIENTED_EDGE('',*,*,#3017,.T.);
#3797=ORIENTED_EDGE('',*,*,#3031,.F.);
#3798=ORIENTED_EDGE('',*,*,#3032,.F.);
#3799=ORIENTED_EDGE('',*,*,#3033,.T.);
#3800=ORIENTED_EDGE('',*,*,#3021,.T.);
#3801=ORIENTED_EDGE('',*,*,#3033,.F.);
#3802=ORIENTED_EDGE('',*,*,#3034,.F.);
#3803=ORIENTED_EDGE('',*,*,#3035,.T.);
#3804=ORIENTED_EDGE('',*,*,#3025,.T.);
#3805=ORIENTED_EDGE('',*,*,#3035,.F.);
#3806=ORIENTED_EDGE('',*,*,#3036,.F.);
#3807=ORIENTED_EDGE('',*,*,#3037,.T.);
#3808=ORIENTED_EDGE('',*,*,#3029,.T.);
#3809=ORIENTED_EDGE('',*,*,#3037,.F.);
#3810=ORIENTED_EDGE('',*,*,#3036,.T.);
#3811=ORIENTED_EDGE('',*,*,#3038,.T.);
#3812=ORIENTED_EDGE('',*,*,#3034,.T.);
#3813=ORIENTED_EDGE('',*,*,#3039,.T.);
#3814=ORIENTED_EDGE('',*,*,#3032,.T.);
#3815=ORIENTED_EDGE('',*,*,#3040,.T.);
#3816=ORIENTED_EDGE('',*,*,#3030,.T.);
#3817=ORIENTED_EDGE('',*,*,#3041,.T.);
#3818=ORIENTED_EDGE('',*,*,#3011,.T.);
#3819=ORIENTED_EDGE('',*,*,#2992,.T.);
#3820=ORIENTED_EDGE('',*,*,#3042,.T.);
#3821=ORIENTED_EDGE('',*,*,#3043,.T.);
#3822=ORIENTED_EDGE('',*,*,#3044,.F.);
#3823=ORIENTED_EDGE('',*,*,#3045,.T.);
#3824=ORIENTED_EDGE('',*,*,#3046,.F.);
#3825=ORIENTED_EDGE('',*,*,#3043,.F.);
#3826=ORIENTED_EDGE('',*,*,#3047,.F.);
#3827=ORIENTED_EDGE('',*,*,#3048,.T.);
#3828=ORIENTED_EDGE('',*,*,#3049,.F.);
#3829=ORIENTED_EDGE('',*,*,#3048,.F.);
#3830=ORIENTED_EDGE('',*,*,#3050,.F.);
#3831=ORIENTED_EDGE('',*,*,#3051,.T.);
#3832=ORIENTED_EDGE('',*,*,#3052,.F.);
#3833=ORIENTED_EDGE('',*,*,#3053,.T.);
#3834=ORIENTED_EDGE('',*,*,#2994,.F.);
#3835=ORIENTED_EDGE('',*,*,#3053,.F.);
#3836=ORIENTED_EDGE('',*,*,#3054,.F.);
#3837=ORIENTED_EDGE('',*,*,#3055,.T.);
#3838=ORIENTED_EDGE('',*,*,#3013,.F.);
#3839=ORIENTED_EDGE('',*,*,#3055,.F.);
#3840=ORIENTED_EDGE('',*,*,#3056,.T.);
#3841=ORIENTED_EDGE('',*,*,#3050,.T.);
#3842=ORIENTED_EDGE('',*,*,#3047,.T.);
#3843=ORIENTED_EDGE('',*,*,#3042,.F.);
#3844=ORIENTED_EDGE('',*,*,#3020,.T.);
#3845=ORIENTED_EDGE('',*,*,#3024,.T.);
#3846=ORIENTED_EDGE('',*,*,#3028,.T.);
#3847=ORIENTED_EDGE('',*,*,#2978,.T.);
#3848=ORIENTED_EDGE('',*,*,#2981,.T.);
#3849=ORIENTED_EDGE('',*,*,#2984,.T.);
#3850=ORIENTED_EDGE('',*,*,#2987,.T.);
#3851=ORIENTED_EDGE('',*,*,#2990,.T.);
#3852=ORIENTED_EDGE('',*,*,#3009,.T.);
#3853=ORIENTED_EDGE('',*,*,#3006,.T.);
#3854=ORIENTED_EDGE('',*,*,#3003,.T.);
#3855=ORIENTED_EDGE('',*,*,#3000,.T.);
#3856=ORIENTED_EDGE('',*,*,#2997,.T.);
#3857=ORIENTED_EDGE('',*,*,#3016,.T.);
#3858=ORIENTED_EDGE('',*,*,#3057,.F.);
#3859=ORIENTED_EDGE('',*,*,#3051,.F.);
#3860=ORIENTED_EDGE('',*,*,#3056,.F.);
#3861=ORIENTED_EDGE('',*,*,#3045,.F.);
#3862=ORIENTED_EDGE('',*,*,#3054,.T.);
#3863=ORIENTED_EDGE('',*,*,#3052,.T.);
#3864=ORIENTED_EDGE('',*,*,#3058,.F.);
#3865=ORIENTED_EDGE('',*,*,#3059,.T.);
#3866=ORIENTED_EDGE('',*,*,#3060,.F.);
#3867=ORIENTED_EDGE('',*,*,#3059,.F.);
#3868=ORIENTED_EDGE('',*,*,#3061,.F.);
#3869=ORIENTED_EDGE('',*,*,#3062,.T.);
#3870=ORIENTED_EDGE('',*,*,#3063,.F.);
#3871=ORIENTED_EDGE('',*,*,#3062,.F.);
#3872=ORIENTED_EDGE('',*,*,#3064,.F.);
#3873=ORIENTED_EDGE('',*,*,#3065,.T.);
#3874=ORIENTED_EDGE('',*,*,#3066,.F.);
#3875=ORIENTED_EDGE('',*,*,#3065,.F.);
#3876=ORIENTED_EDGE('',*,*,#3067,.F.);
#3877=ORIENTED_EDGE('',*,*,#3068,.T.);
#3878=ORIENTED_EDGE('',*,*,#3069,.F.);
#3879=ORIENTED_EDGE('',*,*,#3068,.F.);
#3880=ORIENTED_EDGE('',*,*,#3070,.T.);
#3881=ORIENTED_EDGE('',*,*,#3071,.T.);
#3882=ORIENTED_EDGE('',*,*,#3072,.F.);
#3883=ORIENTED_EDGE('',*,*,#3073,.F.);
#3884=ORIENTED_EDGE('',*,*,#3074,.T.);
#3885=ORIENTED_EDGE('',*,*,#3073,.T.);
#3886=ORIENTED_EDGE('',*,*,#3075,.F.);
#3887=ORIENTED_EDGE('',*,*,#3076,.F.);
#3888=ORIENTED_EDGE('',*,*,#3077,.T.);
#3889=ORIENTED_EDGE('',*,*,#3076,.T.);
#3890=ORIENTED_EDGE('',*,*,#3078,.F.);
#3891=ORIENTED_EDGE('',*,*,#3079,.F.);
#3892=ORIENTED_EDGE('',*,*,#3080,.T.);
#3893=ORIENTED_EDGE('',*,*,#3079,.T.);
#3894=ORIENTED_EDGE('',*,*,#3081,.F.);
#3895=ORIENTED_EDGE('',*,*,#3071,.F.);
#3896=ORIENTED_EDGE('',*,*,#3082,.F.);
#3897=ORIENTED_EDGE('',*,*,#3083,.T.);
#3898=ORIENTED_EDGE('',*,*,#3041,.F.);
#3899=ORIENTED_EDGE('',*,*,#3083,.F.);
#3900=ORIENTED_EDGE('',*,*,#3084,.F.);
#3901=ORIENTED_EDGE('',*,*,#3085,.T.);
#3902=ORIENTED_EDGE('',*,*,#3040,.F.);
#3903=ORIENTED_EDGE('',*,*,#3085,.F.);
#3904=ORIENTED_EDGE('',*,*,#3086,.F.);
#3905=ORIENTED_EDGE('',*,*,#3087,.T.);
#3906=ORIENTED_EDGE('',*,*,#3039,.F.);
#3907=ORIENTED_EDGE('',*,*,#3087,.F.);
#3908=ORIENTED_EDGE('',*,*,#3088,.F.);
#3909=ORIENTED_EDGE('',*,*,#3089,.T.);
#3910=ORIENTED_EDGE('',*,*,#3038,.F.);
#3911=ORIENTED_EDGE('',*,*,#3089,.F.);
#3912=ORIENTED_EDGE('',*,*,#3078,.T.);
#3913=ORIENTED_EDGE('',*,*,#3075,.T.);
#3914=ORIENTED_EDGE('',*,*,#3072,.T.);
#3915=ORIENTED_EDGE('',*,*,#3081,.T.);
#3916=ORIENTED_EDGE('',*,*,#3057,.T.);
#3917=ORIENTED_EDGE('',*,*,#3044,.T.);
#3918=ORIENTED_EDGE('',*,*,#3046,.T.);
#3919=ORIENTED_EDGE('',*,*,#3049,.T.);
#3920=ORIENTED_EDGE('',*,*,#3069,.T.);
#3921=ORIENTED_EDGE('',*,*,#3066,.T.);
#3922=ORIENTED_EDGE('',*,*,#3063,.T.);
#3923=ORIENTED_EDGE('',*,*,#3060,.T.);
#3924=ORIENTED_EDGE('',*,*,#3070,.F.);
#3925=ORIENTED_EDGE('',*,*,#3074,.F.);
#3926=ORIENTED_EDGE('',*,*,#3077,.F.);
#3927=ORIENTED_EDGE('',*,*,#3080,.F.);
#3928=ORIENTED_EDGE('',*,*,#3088,.T.);
#3929=ORIENTED_EDGE('',*,*,#3086,.T.);
#3930=ORIENTED_EDGE('',*,*,#3084,.T.);
#3931=ORIENTED_EDGE('',*,*,#3082,.T.);
#3932=ORIENTED_EDGE('',*,*,#3067,.T.);
#3933=ORIENTED_EDGE('',*,*,#3064,.T.);
#3934=ORIENTED_EDGE('',*,*,#3061,.T.);
#3935=ORIENTED_EDGE('',*,*,#3058,.T.);
#3936=ORIENTED_EDGE('',*,*,#3090,.T.);
#3937=ORIENTED_EDGE('',*,*,#3091,.T.);
#3938=ORIENTED_EDGE('',*,*,#3092,.F.);
#3939=ORIENTED_EDGE('',*,*,#3093,.F.);
#3940=ORIENTED_EDGE('',*,*,#3094,.T.);
#3941=ORIENTED_EDGE('',*,*,#3093,.T.);
#3942=ORIENTED_EDGE('',*,*,#3095,.F.);
#3943=ORIENTED_EDGE('',*,*,#3096,.F.);
#3944=ORIENTED_EDGE('',*,*,#3097,.T.);
#3945=ORIENTED_EDGE('',*,*,#3096,.T.);
#3946=ORIENTED_EDGE('',*,*,#3098,.F.);
#3947=ORIENTED_EDGE('',*,*,#3099,.F.);
#3948=ORIENTED_EDGE('',*,*,#3100,.T.);
#3949=ORIENTED_EDGE('',*,*,#3099,.T.);
#3950=ORIENTED_EDGE('',*,*,#3101,.F.);
#3951=ORIENTED_EDGE('',*,*,#3091,.F.);
#3952=ORIENTED_EDGE('',*,*,#3101,.T.);
#3953=ORIENTED_EDGE('',*,*,#3098,.T.);
#3954=ORIENTED_EDGE('',*,*,#3095,.T.);
#3955=ORIENTED_EDGE('',*,*,#3092,.T.);
#3956=ORIENTED_EDGE('',*,*,#3100,.F.);
#3957=ORIENTED_EDGE('',*,*,#3090,.F.);
#3958=ORIENTED_EDGE('',*,*,#3094,.F.);
#3959=ORIENTED_EDGE('',*,*,#3097,.F.);
#3960=ORIENTED_EDGE('',*,*,#3102,.T.);
#3961=ORIENTED_EDGE('',*,*,#3103,.T.);
#3962=ORIENTED_EDGE('',*,*,#3104,.F.);
#3963=ORIENTED_EDGE('',*,*,#3105,.F.);
#3964=ORIENTED_EDGE('',*,*,#3106,.T.);
#3965=ORIENTED_EDGE('',*,*,#3105,.T.);
#3966=ORIENTED_EDGE('',*,*,#3107,.F.);
#3967=ORIENTED_EDGE('',*,*,#3108,.F.);
#3968=ORIENTED_EDGE('',*,*,#3109,.T.);
#3969=ORIENTED_EDGE('',*,*,#3108,.T.);
#3970=ORIENTED_EDGE('',*,*,#3110,.F.);
#3971=ORIENTED_EDGE('',*,*,#3111,.F.);
#3972=ORIENTED_EDGE('',*,*,#3112,.T.);
#3973=ORIENTED_EDGE('',*,*,#3111,.T.);
#3974=ORIENTED_EDGE('',*,*,#3113,.F.);
#3975=ORIENTED_EDGE('',*,*,#3103,.F.);
#3976=ORIENTED_EDGE('',*,*,#3113,.T.);
#3977=ORIENTED_EDGE('',*,*,#3110,.T.);
#3978=ORIENTED_EDGE('',*,*,#3107,.T.);
#3979=ORIENTED_EDGE('',*,*,#3104,.T.);
#3980=ORIENTED_EDGE('',*,*,#3112,.F.);
#3981=ORIENTED_EDGE('',*,*,#3102,.F.);
#3982=ORIENTED_EDGE('',*,*,#3106,.F.);
#3983=ORIENTED_EDGE('',*,*,#3109,.F.);
#3984=ORIENTED_EDGE('',*,*,#3114,.F.);
#3985=ORIENTED_EDGE('',*,*,#3115,.F.);
#3986=ORIENTED_EDGE('',*,*,#3116,.F.);
#3987=ORIENTED_EDGE('',*,*,#3117,.F.);
#3988=ORIENTED_EDGE('',*,*,#3118,.F.);
#3989=ORIENTED_EDGE('',*,*,#3115,.T.);
#3990=ORIENTED_EDGE('',*,*,#3119,.F.);
#3991=ORIENTED_EDGE('',*,*,#3120,.F.);
#3992=ORIENTED_EDGE('',*,*,#3121,.F.);
#3993=ORIENTED_EDGE('',*,*,#3122,.T.);
#3994=ORIENTED_EDGE('',*,*,#3123,.F.);
#3995=ORIENTED_EDGE('',*,*,#3124,.F.);
#3996=ORIENTED_EDGE('',*,*,#3125,.F.);
#3997=ORIENTED_EDGE('',*,*,#3126,.F.);
#3998=ORIENTED_EDGE('',*,*,#3122,.F.);
#3999=ORIENTED_EDGE('',*,*,#3127,.F.);
#4000=ORIENTED_EDGE('',*,*,#3128,.T.);
#4001=ORIENTED_EDGE('',*,*,#3129,.F.);
#4002=ORIENTED_EDGE('',*,*,#3130,.F.);
#4003=ORIENTED_EDGE('',*,*,#3131,.F.);
#4004=ORIENTED_EDGE('',*,*,#3132,.F.);
#4005=ORIENTED_EDGE('',*,*,#3128,.F.);
#4006=ORIENTED_EDGE('',*,*,#3133,.F.);
#4007=ORIENTED_EDGE('',*,*,#3134,.T.);
#4008=ORIENTED_EDGE('',*,*,#3135,.F.);
#4009=ORIENTED_EDGE('',*,*,#3136,.F.);
#4010=ORIENTED_EDGE('',*,*,#3137,.F.);
#4011=ORIENTED_EDGE('',*,*,#3138,.F.);
#4012=ORIENTED_EDGE('',*,*,#3134,.F.);
#4013=ORIENTED_EDGE('',*,*,#3117,.T.);
#4014=ORIENTED_EDGE('',*,*,#3139,.T.);
#4015=ORIENTED_EDGE('',*,*,#3137,.T.);
#4016=ORIENTED_EDGE('',*,*,#3140,.T.);
#4017=ORIENTED_EDGE('',*,*,#3131,.T.);
#4018=ORIENTED_EDGE('',*,*,#3141,.T.);
#4019=ORIENTED_EDGE('',*,*,#3125,.T.);
#4020=ORIENTED_EDGE('',*,*,#3142,.T.);
#4021=ORIENTED_EDGE('',*,*,#3143,.T.);
#4022=ORIENTED_EDGE('',*,*,#3144,.F.);
#4023=ORIENTED_EDGE('',*,*,#3145,.T.);
#4024=ORIENTED_EDGE('',*,*,#3120,.T.);
#4025=ORIENTED_EDGE('',*,*,#3145,.F.);
#4026=ORIENTED_EDGE('',*,*,#3146,.F.);
#4027=ORIENTED_EDGE('',*,*,#3147,.T.);
#4028=ORIENTED_EDGE('',*,*,#3123,.T.);
#4029=ORIENTED_EDGE('',*,*,#3147,.F.);
#4030=ORIENTED_EDGE('',*,*,#3148,.F.);
#4031=ORIENTED_EDGE('',*,*,#3149,.T.);
#4032=ORIENTED_EDGE('',*,*,#3129,.T.);
#4033=ORIENTED_EDGE('',*,*,#3149,.F.);
#4034=ORIENTED_EDGE('',*,*,#3150,.F.);
#4035=ORIENTED_EDGE('',*,*,#3151,.T.);
#4036=ORIENTED_EDGE('',*,*,#3135,.T.);
#4037=ORIENTED_EDGE('',*,*,#3151,.F.);
#4038=ORIENTED_EDGE('',*,*,#3152,.F.);
#4039=ORIENTED_EDGE('',*,*,#3153,.T.);
#4040=ORIENTED_EDGE('',*,*,#3154,.T.);
#4041=ORIENTED_EDGE('',*,*,#3153,.F.);
#4042=ORIENTED_EDGE('',*,*,#3154,.F.);
#4043=ORIENTED_EDGE('',*,*,#3155,.F.);
#4044=ORIENTED_EDGE('',*,*,#3143,.F.);
#4045=ORIENTED_EDGE('',*,*,#3156,.T.);
#4046=ORIENTED_EDGE('',*,*,#3155,.T.);
#4047=ORIENTED_EDGE('',*,*,#3156,.F.);
#4048=ORIENTED_EDGE('',*,*,#3114,.T.);
#4049=ORIENTED_EDGE('',*,*,#3142,.F.);
#4050=ORIENTED_EDGE('',*,*,#3124,.T.);
#4051=ORIENTED_EDGE('',*,*,#3121,.T.);
#4052=ORIENTED_EDGE('',*,*,#3126,.T.);
#4053=ORIENTED_EDGE('',*,*,#3141,.F.);
#4054=ORIENTED_EDGE('',*,*,#3130,.T.);
#4055=ORIENTED_EDGE('',*,*,#3127,.T.);
#4056=ORIENTED_EDGE('',*,*,#3132,.T.);
#4057=ORIENTED_EDGE('',*,*,#3140,.F.);
#4058=ORIENTED_EDGE('',*,*,#3136,.T.);
#4059=ORIENTED_EDGE('',*,*,#3133,.T.);
#4060=ORIENTED_EDGE('',*,*,#3138,.T.);
#4061=ORIENTED_EDGE('',*,*,#3139,.F.);
#4062=ORIENTED_EDGE('',*,*,#3116,.T.);
#4063=ORIENTED_EDGE('',*,*,#3118,.T.);
#4064=ORIENTED_EDGE('',*,*,#3157,.T.);
#4065=ORIENTED_EDGE('',*,*,#3158,.T.);
#4066=ORIENTED_EDGE('',*,*,#3157,.F.);
#4067=ORIENTED_EDGE('',*,*,#3119,.T.);
#4068=ORIENTED_EDGE('',*,*,#3158,.F.);
#4069=ORIENTED_EDGE('',*,*,#3152,.T.);
#4070=ORIENTED_EDGE('',*,*,#3150,.T.);
#4071=ORIENTED_EDGE('',*,*,#3148,.T.);
#4072=ORIENTED_EDGE('',*,*,#3146,.T.);
#4073=ORIENTED_EDGE('',*,*,#3144,.T.);
#4074=ORIENTED_EDGE('',*,*,#3159,.F.);
#4075=ORIENTED_EDGE('',*,*,#3160,.F.);
#4076=ORIENTED_EDGE('',*,*,#3161,.F.);
#4077=ORIENTED_EDGE('',*,*,#3162,.F.);
#4078=ORIENTED_EDGE('',*,*,#3163,.F.);
#4079=ORIENTED_EDGE('',*,*,#3160,.T.);
#4080=ORIENTED_EDGE('',*,*,#3164,.F.);
#4081=ORIENTED_EDGE('',*,*,#3165,.F.);
#4082=ORIENTED_EDGE('',*,*,#3166,.F.);
#4083=ORIENTED_EDGE('',*,*,#3167,.T.);
#4084=ORIENTED_EDGE('',*,*,#3168,.F.);
#4085=ORIENTED_EDGE('',*,*,#3169,.F.);
#4086=ORIENTED_EDGE('',*,*,#3170,.F.);
#4087=ORIENTED_EDGE('',*,*,#3171,.F.);
#4088=ORIENTED_EDGE('',*,*,#3167,.F.);
#4089=ORIENTED_EDGE('',*,*,#3172,.F.);
#4090=ORIENTED_EDGE('',*,*,#3173,.T.);
#4091=ORIENTED_EDGE('',*,*,#3174,.F.);
#4092=ORIENTED_EDGE('',*,*,#3175,.F.);
#4093=ORIENTED_EDGE('',*,*,#3176,.F.);
#4094=ORIENTED_EDGE('',*,*,#3177,.F.);
#4095=ORIENTED_EDGE('',*,*,#3173,.F.);
#4096=ORIENTED_EDGE('',*,*,#3178,.F.);
#4097=ORIENTED_EDGE('',*,*,#3179,.T.);
#4098=ORIENTED_EDGE('',*,*,#3180,.F.);
#4099=ORIENTED_EDGE('',*,*,#3181,.F.);
#4100=ORIENTED_EDGE('',*,*,#3182,.F.);
#4101=ORIENTED_EDGE('',*,*,#3183,.F.);
#4102=ORIENTED_EDGE('',*,*,#3179,.F.);
#4103=ORIENTED_EDGE('',*,*,#3162,.T.);
#4104=ORIENTED_EDGE('',*,*,#3184,.T.);
#4105=ORIENTED_EDGE('',*,*,#3182,.T.);
#4106=ORIENTED_EDGE('',*,*,#3185,.T.);
#4107=ORIENTED_EDGE('',*,*,#3176,.T.);
#4108=ORIENTED_EDGE('',*,*,#3186,.T.);
#4109=ORIENTED_EDGE('',*,*,#3170,.T.);
#4110=ORIENTED_EDGE('',*,*,#3187,.T.);
#4111=ORIENTED_EDGE('',*,*,#3188,.T.);
#4112=ORIENTED_EDGE('',*,*,#3189,.F.);
#4113=ORIENTED_EDGE('',*,*,#3190,.T.);
#4114=ORIENTED_EDGE('',*,*,#3165,.T.);
#4115=ORIENTED_EDGE('',*,*,#3190,.F.);
#4116=ORIENTED_EDGE('',*,*,#3191,.F.);
#4117=ORIENTED_EDGE('',*,*,#3192,.T.);
#4118=ORIENTED_EDGE('',*,*,#3168,.T.);
#4119=ORIENTED_EDGE('',*,*,#3192,.F.);
#4120=ORIENTED_EDGE('',*,*,#3193,.F.);
#4121=ORIENTED_EDGE('',*,*,#3194,.T.);
#4122=ORIENTED_EDGE('',*,*,#3174,.T.);
#4123=ORIENTED_EDGE('',*,*,#3194,.F.);
#4124=ORIENTED_EDGE('',*,*,#3195,.F.);
#4125=ORIENTED_EDGE('',*,*,#3196,.T.);
#4126=ORIENTED_EDGE('',*,*,#3180,.T.);
#4127=ORIENTED_EDGE('',*,*,#3196,.F.);
#4128=ORIENTED_EDGE('',*,*,#3197,.F.);
#4129=ORIENTED_EDGE('',*,*,#3198,.T.);
#4130=ORIENTED_EDGE('',*,*,#3199,.T.);
#4131=ORIENTED_EDGE('',*,*,#3198,.F.);
#4132=ORIENTED_EDGE('',*,*,#3199,.F.);
#4133=ORIENTED_EDGE('',*,*,#3200,.F.);
#4134=ORIENTED_EDGE('',*,*,#3188,.F.);
#4135=ORIENTED_EDGE('',*,*,#3201,.T.);
#4136=ORIENTED_EDGE('',*,*,#3200,.T.);
#4137=ORIENTED_EDGE('',*,*,#3201,.F.);
#4138=ORIENTED_EDGE('',*,*,#3159,.T.);
#4139=ORIENTED_EDGE('',*,*,#3187,.F.);
#4140=ORIENTED_EDGE('',*,*,#3169,.T.);
#4141=ORIENTED_EDGE('',*,*,#3166,.T.);
#4142=ORIENTED_EDGE('',*,*,#3171,.T.);
#4143=ORIENTED_EDGE('',*,*,#3186,.F.);
#4144=ORIENTED_EDGE('',*,*,#3175,.T.);
#4145=ORIENTED_EDGE('',*,*,#3172,.T.);
#4146=ORIENTED_EDGE('',*,*,#3177,.T.);
#4147=ORIENTED_EDGE('',*,*,#3185,.F.);
#4148=ORIENTED_EDGE('',*,*,#3181,.T.);
#4149=ORIENTED_EDGE('',*,*,#3178,.T.);
#4150=ORIENTED_EDGE('',*,*,#3183,.T.);
#4151=ORIENTED_EDGE('',*,*,#3184,.F.);
#4152=ORIENTED_EDGE('',*,*,#3161,.T.);
#4153=ORIENTED_EDGE('',*,*,#3163,.T.);
#4154=ORIENTED_EDGE('',*,*,#3202,.T.);
#4155=ORIENTED_EDGE('',*,*,#3203,.T.);
#4156=ORIENTED_EDGE('',*,*,#3202,.F.);
#4157=ORIENTED_EDGE('',*,*,#3164,.T.);
#4158=ORIENTED_EDGE('',*,*,#3203,.F.);
#4159=ORIENTED_EDGE('',*,*,#3197,.T.);
#4160=ORIENTED_EDGE('',*,*,#3195,.T.);
#4161=ORIENTED_EDGE('',*,*,#3193,.T.);
#4162=ORIENTED_EDGE('',*,*,#3191,.T.);
#4163=ORIENTED_EDGE('',*,*,#3189,.T.);
#4164=ORIENTED_EDGE('',*,*,#3204,.F.);
#4165=ORIENTED_EDGE('',*,*,#3205,.F.);
#4166=ORIENTED_EDGE('',*,*,#3206,.T.);
#4167=ORIENTED_EDGE('',*,*,#3204,.T.);
#4168=ORIENTED_EDGE('',*,*,#3206,.F.);
#4169=ORIENTED_EDGE('',*,*,#3207,.F.);
#4170=ORIENTED_EDGE('',*,*,#3208,.T.);
#4171=ORIENTED_EDGE('',*,*,#3205,.T.);
#4172=ORIENTED_EDGE('',*,*,#3208,.F.);
#4173=ORIENTED_EDGE('',*,*,#3209,.F.);
#4174=ORIENTED_EDGE('',*,*,#3210,.T.);
#4175=ORIENTED_EDGE('',*,*,#3207,.T.);
#4176=ORIENTED_EDGE('',*,*,#3210,.F.);
#4177=ORIENTED_EDGE('',*,*,#3209,.T.);
#4178=ORIENTED_EDGE('',*,*,#3211,.F.);
#4179=ORIENTED_EDGE('',*,*,#3212,.F.);
#4180=ORIENTED_EDGE('',*,*,#3213,.T.);
#4181=ORIENTED_EDGE('',*,*,#3211,.T.);
#4182=ORIENTED_EDGE('',*,*,#3213,.F.);
#4183=ORIENTED_EDGE('',*,*,#3214,.F.);
#4184=ORIENTED_EDGE('',*,*,#3215,.T.);
#4185=ORIENTED_EDGE('',*,*,#3212,.T.);
#4186=ORIENTED_EDGE('',*,*,#3215,.F.);
#4187=ORIENTED_EDGE('',*,*,#3216,.F.);
#4188=ORIENTED_EDGE('',*,*,#3217,.T.);
#4189=ORIENTED_EDGE('',*,*,#3214,.T.);
#4190=ORIENTED_EDGE('',*,*,#3217,.F.);
#4191=ORIENTED_EDGE('',*,*,#3216,.T.);
#4192=ORIENTED_EDGE('',*,*,#3218,.T.);
#4193=ORIENTED_EDGE('',*,*,#3219,.T.);
#4194=ORIENTED_EDGE('',*,*,#3220,.T.);
#4195=ORIENTED_EDGE('',*,*,#3221,.F.);
#4196=ORIENTED_EDGE('',*,*,#3222,.T.);
#4197=ORIENTED_EDGE('',*,*,#3223,.T.);
#4198=ORIENTED_EDGE('',*,*,#3224,.T.);
#4199=ORIENTED_EDGE('',*,*,#3219,.F.);
#4200=ORIENTED_EDGE('',*,*,#3225,.T.);
#4201=ORIENTED_EDGE('',*,*,#3226,.T.);
#4202=ORIENTED_EDGE('',*,*,#3227,.T.);
#4203=ORIENTED_EDGE('',*,*,#3223,.F.);
#4204=ORIENTED_EDGE('',*,*,#3228,.T.);
#4205=ORIENTED_EDGE('',*,*,#3229,.T.);
#4206=ORIENTED_EDGE('',*,*,#3230,.T.);
#4207=ORIENTED_EDGE('',*,*,#3226,.F.);
#4208=ORIENTED_EDGE('',*,*,#3231,.T.);
#4209=ORIENTED_EDGE('',*,*,#3232,.T.);
#4210=ORIENTED_EDGE('',*,*,#3233,.T.);
#4211=ORIENTED_EDGE('',*,*,#3229,.F.);
#4212=ORIENTED_EDGE('',*,*,#3234,.T.);
#4213=ORIENTED_EDGE('',*,*,#3221,.T.);
#4214=ORIENTED_EDGE('',*,*,#3235,.T.);
#4215=ORIENTED_EDGE('',*,*,#3232,.F.);
#4216=ORIENTED_EDGE('',*,*,#3234,.F.);
#4217=ORIENTED_EDGE('',*,*,#3231,.F.);
#4218=ORIENTED_EDGE('',*,*,#3228,.F.);
#4219=ORIENTED_EDGE('',*,*,#3225,.F.);
#4220=ORIENTED_EDGE('',*,*,#3222,.F.);
#4221=ORIENTED_EDGE('',*,*,#3218,.F.);
#4222=ORIENTED_EDGE('',*,*,#3235,.F.);
#4223=ORIENTED_EDGE('',*,*,#3220,.F.);
#4224=ORIENTED_EDGE('',*,*,#3224,.F.);
#4225=ORIENTED_EDGE('',*,*,#3227,.F.);
#4226=ORIENTED_EDGE('',*,*,#3230,.F.);
#4227=ORIENTED_EDGE('',*,*,#3233,.F.);
#4228=ORIENTED_EDGE('',*,*,#3236,.F.);
#4229=ORIENTED_EDGE('',*,*,#3237,.F.);
#4230=ORIENTED_EDGE('',*,*,#3238,.T.);
#4231=ORIENTED_EDGE('',*,*,#3239,.F.);
#4232=ORIENTED_EDGE('',*,*,#3240,.F.);
#4233=ORIENTED_EDGE('',*,*,#3238,.F.);
#4234=ORIENTED_EDGE('',*,*,#3239,.T.);
#4235=ORIENTED_EDGE('',*,*,#3240,.T.);
#4236=ORIENTED_EDGE('',*,*,#3241,.T.);
#4237=ORIENTED_EDGE('',*,*,#3242,.T.);
#4238=ORIENTED_EDGE('',*,*,#3241,.F.);
#4239=ORIENTED_EDGE('',*,*,#3243,.T.);
#4240=ORIENTED_EDGE('',*,*,#3244,.T.);
#4241=ORIENTED_EDGE('',*,*,#3245,.F.);
#4242=ORIENTED_EDGE('',*,*,#3244,.F.);
#4243=ORIENTED_EDGE('',*,*,#3245,.T.);
#4244=ORIENTED_EDGE('',*,*,#3246,.T.);
#4245=ORIENTED_EDGE('',*,*,#3247,.F.);
#4246=ORIENTED_EDGE('',*,*,#3246,.F.);
#4247=ORIENTED_EDGE('',*,*,#3242,.F.);
#4248=ORIENTED_EDGE('',*,*,#3247,.T.);
#4249=ORIENTED_EDGE('',*,*,#3248,.F.);
#4250=ORIENTED_EDGE('',*,*,#3249,.T.);
#4251=ORIENTED_EDGE('',*,*,#3236,.T.);
#4252=ORIENTED_EDGE('',*,*,#3237,.T.);
#4253=ORIENTED_EDGE('',*,*,#3249,.F.);
#4254=ORIENTED_EDGE('',*,*,#3248,.T.);
#4255=ORIENTED_EDGE('',*,*,#3250,.F.);
#4256=ORIENTED_EDGE('',*,*,#3250,.T.);
#4257=ORIENTED_EDGE('',*,*,#3251,.T.);
#4258=ORIENTED_EDGE('',*,*,#3243,.F.);
#4259=ORIENTED_EDGE('',*,*,#3251,.F.);
#4260=ORIENTED_EDGE('',*,*,#3252,.F.);
#4261=ORIENTED_EDGE('',*,*,#3253,.F.);
#4262=ORIENTED_EDGE('',*,*,#3254,.T.);
#4263=ORIENTED_EDGE('',*,*,#3255,.F.);
#4264=ORIENTED_EDGE('',*,*,#3256,.F.);
#4265=ORIENTED_EDGE('',*,*,#3254,.F.);
#4266=ORIENTED_EDGE('',*,*,#3257,.T.);
#4267=ORIENTED_EDGE('',*,*,#3258,.T.);
#4268=ORIENTED_EDGE('',*,*,#3255,.T.);
#4269=ORIENTED_EDGE('',*,*,#3256,.T.);
#4270=ORIENTED_EDGE('',*,*,#3258,.F.);
#4271=ORIENTED_EDGE('',*,*,#3259,.F.);
#4272=ORIENTED_EDGE('',*,*,#3260,.T.);
#4273=ORIENTED_EDGE('',*,*,#3261,.F.);
#4274=ORIENTED_EDGE('',*,*,#3262,.T.);
#4275=ORIENTED_EDGE('',*,*,#3259,.T.);
#4276=ORIENTED_EDGE('',*,*,#3262,.F.);
#4277=ORIENTED_EDGE('',*,*,#3263,.F.);
#4278=ORIENTED_EDGE('',*,*,#3264,.T.);
#4279=ORIENTED_EDGE('',*,*,#3261,.T.);
#4280=ORIENTED_EDGE('',*,*,#3264,.F.);
#4281=ORIENTED_EDGE('',*,*,#3265,.F.);
#4282=ORIENTED_EDGE('',*,*,#3266,.T.);
#4283=ORIENTED_EDGE('',*,*,#3263,.T.);
#4284=ORIENTED_EDGE('',*,*,#3266,.F.);
#4285=ORIENTED_EDGE('',*,*,#3265,.T.);
#4286=ORIENTED_EDGE('',*,*,#3257,.F.);
#4287=ORIENTED_EDGE('',*,*,#3252,.T.);
#4288=ORIENTED_EDGE('',*,*,#3253,.T.);
#4289=ORIENTED_EDGE('',*,*,#3267,.T.);
#4290=ORIENTED_EDGE('',*,*,#3260,.F.);
#4291=ORIENTED_EDGE('',*,*,#3267,.F.);
#4292=ORIENTED_EDGE('',*,*,#3268,.T.);
#4293=ORIENTED_EDGE('',*,*,#3268,.F.);
#4294=ORIENTED_EDGE('',*,*,#3269,.T.);
#4295=ORIENTED_EDGE('',*,*,#3269,.F.);
#4296=ORIENTED_EDGE('',*,*,#3270,.T.);
#4297=ORIENTED_EDGE('',*,*,#3270,.F.);
#4298=ORIENTED_EDGE('',*,*,#3271,.T.);
#4299=ORIENTED_EDGE('',*,*,#3271,.F.);
#4300=ORIENTED_EDGE('',*,*,#3272,.T.);
#4301=ORIENTED_EDGE('',*,*,#3272,.F.);
#4302=ORIENTED_EDGE('',*,*,#3273,.T.);
#4303=ORIENTED_EDGE('',*,*,#3273,.F.);
#4304=ORIENTED_EDGE('',*,*,#3274,.T.);
#4305=ORIENTED_EDGE('',*,*,#3274,.F.);
#4306=ORIENTED_EDGE('',*,*,#3275,.T.);
#4307=ORIENTED_EDGE('',*,*,#3275,.F.);
#4308=ORIENTED_EDGE('',*,*,#3276,.F.);
#4309=ORIENTED_EDGE('',*,*,#3277,.F.);
#4310=ORIENTED_EDGE('',*,*,#3278,.F.);
#4311=ORIENTED_EDGE('',*,*,#3279,.F.);
#4312=ORIENTED_EDGE('',*,*,#3278,.T.);
#4313=ORIENTED_EDGE('',*,*,#3280,.F.);
#4314=ORIENTED_EDGE('',*,*,#3281,.T.);
#4315=ORIENTED_EDGE('',*,*,#3282,.F.);
#4316=ORIENTED_EDGE('',*,*,#3283,.T.);
#4317=ORIENTED_EDGE('',*,*,#3284,.F.);
#4318=ORIENTED_EDGE('',*,*,#3285,.T.);
#4319=ORIENTED_EDGE('',*,*,#3286,.T.);
#4320=ORIENTED_EDGE('',*,*,#3287,.F.);
#4321=ORIENTED_EDGE('',*,*,#3286,.F.);
#4322=ORIENTED_EDGE('',*,*,#3288,.T.);
#4323=ORIENTED_EDGE('',*,*,#3289,.F.);
#4324=ORIENTED_EDGE('',*,*,#3290,.T.);
#4325=ORIENTED_EDGE('',*,*,#3291,.F.);
#4326=ORIENTED_EDGE('',*,*,#3292,.T.);
#4327=ORIENTED_EDGE('',*,*,#3293,.F.);
#4328=ORIENTED_EDGE('',*,*,#3294,.T.);
#4329=ORIENTED_EDGE('',*,*,#3295,.F.);
#4330=ORIENTED_EDGE('',*,*,#3296,.T.);
#4331=ORIENTED_EDGE('',*,*,#3297,.F.);
#4332=ORIENTED_EDGE('',*,*,#3277,.T.);
#4333=ORIENTED_EDGE('',*,*,#3298,.T.);
#4334=ORIENTED_EDGE('',*,*,#3299,.T.);
#4335=ORIENTED_EDGE('',*,*,#3280,.T.);
#4336=ORIENTED_EDGE('',*,*,#3300,.F.);
#4337=ORIENTED_EDGE('',*,*,#3301,.F.);
#4338=ORIENTED_EDGE('',*,*,#3281,.F.);
#4339=ORIENTED_EDGE('',*,*,#3299,.F.);
#4340=ORIENTED_EDGE('',*,*,#3301,.T.);
#4341=ORIENTED_EDGE('',*,*,#3302,.T.);
#4342=ORIENTED_EDGE('',*,*,#3303,.T.);
#4343=ORIENTED_EDGE('',*,*,#3282,.T.);
#4344=ORIENTED_EDGE('',*,*,#3304,.F.);
#4345=ORIENTED_EDGE('',*,*,#3305,.F.);
#4346=ORIENTED_EDGE('',*,*,#3283,.F.);
#4347=ORIENTED_EDGE('',*,*,#3303,.F.);
#4348=ORIENTED_EDGE('',*,*,#3305,.T.);
#4349=ORIENTED_EDGE('',*,*,#3306,.T.);
#4350=ORIENTED_EDGE('',*,*,#3307,.T.);
#4351=ORIENTED_EDGE('',*,*,#3284,.T.);
#4352=ORIENTED_EDGE('',*,*,#3308,.F.);
#4353=ORIENTED_EDGE('',*,*,#3309,.F.);
#4354=ORIENTED_EDGE('',*,*,#3288,.F.);
#4355=ORIENTED_EDGE('',*,*,#3285,.F.);
#4356=ORIENTED_EDGE('',*,*,#3307,.F.);
#4357=ORIENTED_EDGE('',*,*,#3310,.F.);
#4358=ORIENTED_EDGE('',*,*,#3309,.T.);
#4359=ORIENTED_EDGE('',*,*,#3311,.T.);
#4360=ORIENTED_EDGE('',*,*,#3312,.T.);
#4361=ORIENTED_EDGE('',*,*,#3289,.T.);
#4362=ORIENTED_EDGE('',*,*,#3313,.F.);
#4363=ORIENTED_EDGE('',*,*,#3314,.F.);
#4364=ORIENTED_EDGE('',*,*,#3290,.F.);
#4365=ORIENTED_EDGE('',*,*,#3312,.F.);
#4366=ORIENTED_EDGE('',*,*,#3314,.T.);
#4367=ORIENTED_EDGE('',*,*,#3315,.T.);
#4368=ORIENTED_EDGE('',*,*,#3316,.T.);
#4369=ORIENTED_EDGE('',*,*,#3291,.T.);
#4370=ORIENTED_EDGE('',*,*,#3317,.F.);
#4371=ORIENTED_EDGE('',*,*,#3318,.F.);
#4372=ORIENTED_EDGE('',*,*,#3292,.F.);
#4373=ORIENTED_EDGE('',*,*,#3316,.F.);
#4374=ORIENTED_EDGE('',*,*,#3318,.T.);
#4375=ORIENTED_EDGE('',*,*,#3319,.T.);
#4376=ORIENTED_EDGE('',*,*,#3320,.T.);
#4377=ORIENTED_EDGE('',*,*,#3293,.T.);
#4378=ORIENTED_EDGE('',*,*,#3294,.F.);
#4379=ORIENTED_EDGE('',*,*,#3320,.F.);
#4380=ORIENTED_EDGE('',*,*,#3321,.F.);
#4381=ORIENTED_EDGE('',*,*,#3322,.F.);
#4382=ORIENTED_EDGE('',*,*,#3323,.F.);
#4383=ORIENTED_EDGE('',*,*,#3324,.T.);
#4384=ORIENTED_EDGE('',*,*,#3310,.T.);
#4385=ORIENTED_EDGE('',*,*,#3306,.F.);
#4386=ORIENTED_EDGE('',*,*,#3304,.T.);
#4387=ORIENTED_EDGE('',*,*,#3302,.F.);
#4388=ORIENTED_EDGE('',*,*,#3300,.T.);
#4389=ORIENTED_EDGE('',*,*,#3298,.F.);
#4390=ORIENTED_EDGE('',*,*,#3276,.T.);
#4391=ORIENTED_EDGE('',*,*,#3325,.F.);
#4392=ORIENTED_EDGE('',*,*,#3326,.T.);
#4393=ORIENTED_EDGE('',*,*,#3327,.F.);
#4394=ORIENTED_EDGE('',*,*,#3321,.T.);
#4395=ORIENTED_EDGE('',*,*,#3319,.F.);
#4396=ORIENTED_EDGE('',*,*,#3317,.T.);
#4397=ORIENTED_EDGE('',*,*,#3315,.F.);
#4398=ORIENTED_EDGE('',*,*,#3313,.T.);
#4399=ORIENTED_EDGE('',*,*,#3311,.F.);
#4400=ORIENTED_EDGE('',*,*,#3308,.T.);
#4401=ORIENTED_EDGE('',*,*,#3324,.F.);
#4402=ORIENTED_EDGE('',*,*,#3279,.T.);
#4403=ORIENTED_EDGE('',*,*,#3297,.T.);
#4404=ORIENTED_EDGE('',*,*,#3328,.T.);
#4405=ORIENTED_EDGE('',*,*,#3325,.T.);
#4406=ORIENTED_EDGE('',*,*,#3296,.F.);
#4407=ORIENTED_EDGE('',*,*,#3329,.F.);
#4408=ORIENTED_EDGE('',*,*,#3326,.F.);
#4409=ORIENTED_EDGE('',*,*,#3328,.F.);
#4410=ORIENTED_EDGE('',*,*,#3287,.T.);
#4411=ORIENTED_EDGE('',*,*,#3323,.T.);
#4412=ORIENTED_EDGE('',*,*,#3322,.T.);
#4413=ORIENTED_EDGE('',*,*,#3327,.T.);
#4414=ORIENTED_EDGE('',*,*,#3329,.T.);
#4415=ORIENTED_EDGE('',*,*,#3295,.T.);
#4416=ORIENTED_EDGE('',*,*,#3330,.F.);
#4417=ORIENTED_EDGE('',*,*,#3331,.T.);
#4418=ORIENTED_EDGE('',*,*,#3332,.F.);
#4419=ORIENTED_EDGE('',*,*,#3333,.T.);
#4420=ORIENTED_EDGE('',*,*,#3330,.T.);
#4421=ORIENTED_EDGE('',*,*,#3333,.F.);
#4422=ORIENTED_EDGE('',*,*,#3332,.T.);
#4423=ORIENTED_EDGE('',*,*,#3334,.F.);
#4424=ORIENTED_EDGE('',*,*,#3334,.T.);
#4425=ORIENTED_EDGE('',*,*,#3335,.T.);
#4426=ORIENTED_EDGE('',*,*,#3331,.F.);
#4427=ORIENTED_EDGE('',*,*,#3335,.F.);
#4428=ORIENTED_EDGE('',*,*,#3336,.F.);
#4429=ORIENTED_EDGE('',*,*,#3337,.T.);
#4430=ORIENTED_EDGE('',*,*,#3338,.F.);
#4431=ORIENTED_EDGE('',*,*,#3339,.T.);
#4432=ORIENTED_EDGE('',*,*,#3336,.T.);
#4433=ORIENTED_EDGE('',*,*,#3339,.F.);
#4434=ORIENTED_EDGE('',*,*,#3338,.T.);
#4435=ORIENTED_EDGE('',*,*,#3340,.F.);
#4436=ORIENTED_EDGE('',*,*,#3340,.T.);
#4437=ORIENTED_EDGE('',*,*,#3341,.T.);
#4438=ORIENTED_EDGE('',*,*,#3337,.F.);
#4439=ORIENTED_EDGE('',*,*,#3341,.F.);
#4440=ORIENTED_EDGE('',*,*,#3342,.F.);
#4441=ORIENTED_EDGE('',*,*,#3343,.T.);
#4442=ORIENTED_EDGE('',*,*,#3344,.F.);
#4443=ORIENTED_EDGE('',*,*,#3343,.F.);
#4444=ORIENTED_EDGE('',*,*,#3342,.T.);
#4445=ORIENTED_EDGE('',*,*,#3345,.F.);
#4446=ORIENTED_EDGE('',*,*,#3346,.T.);
#4447=ORIENTED_EDGE('',*,*,#3347,.F.);
#4448=ORIENTED_EDGE('',*,*,#3346,.F.);
#4449=ORIENTED_EDGE('',*,*,#3348,.T.);
#4450=ORIENTED_EDGE('',*,*,#3349,.F.);
#4451=ORIENTED_EDGE('',*,*,#3350,.F.);
#4452=ORIENTED_EDGE('',*,*,#3351,.T.);
#4453=ORIENTED_EDGE('',*,*,#3352,.F.);
#4454=ORIENTED_EDGE('',*,*,#3353,.F.);
#4455=ORIENTED_EDGE('',*,*,#3354,.F.);
#4456=ORIENTED_EDGE('',*,*,#3355,.F.);
#4457=ORIENTED_EDGE('',*,*,#3356,.F.);
#4458=ORIENTED_EDGE('',*,*,#3357,.F.);
#4459=ORIENTED_EDGE('',*,*,#3358,.F.);
#4460=ORIENTED_EDGE('',*,*,#3351,.F.);
#4461=ORIENTED_EDGE('',*,*,#3345,.T.);
#4462=ORIENTED_EDGE('',*,*,#3359,.T.);
#4463=ORIENTED_EDGE('',*,*,#3360,.F.);
#4464=ORIENTED_EDGE('',*,*,#3361,.F.);
#4465=ORIENTED_EDGE('',*,*,#3348,.F.);
#4466=ORIENTED_EDGE('',*,*,#3358,.T.);
#4467=ORIENTED_EDGE('',*,*,#3362,.F.);
#4468=ORIENTED_EDGE('',*,*,#3352,.T.);
#4469=ORIENTED_EDGE('',*,*,#3350,.T.);
#4470=ORIENTED_EDGE('',*,*,#3363,.F.);
#4471=ORIENTED_EDGE('',*,*,#3364,.F.);
#4472=ORIENTED_EDGE('',*,*,#3365,.F.);
#4473=ORIENTED_EDGE('',*,*,#3366,.F.);
#4474=ORIENTED_EDGE('',*,*,#3354,.T.);
#4475=ORIENTED_EDGE('',*,*,#3367,.F.);
#4476=ORIENTED_EDGE('',*,*,#3356,.T.);
#4477=ORIENTED_EDGE('',*,*,#3368,.T.);
#4478=ORIENTED_EDGE('',*,*,#3369,.F.);
#4479=ORIENTED_EDGE('',*,*,#3355,.T.);
#4480=ORIENTED_EDGE('',*,*,#3366,.T.);
#4481=ORIENTED_EDGE('',*,*,#3370,.F.);
#4482=ORIENTED_EDGE('',*,*,#3368,.F.);
#4483=ORIENTED_EDGE('',*,*,#3361,.T.);
#4484=ORIENTED_EDGE('',*,*,#3371,.T.);
#4485=ORIENTED_EDGE('',*,*,#3369,.T.);
#4486=ORIENTED_EDGE('',*,*,#3370,.T.);
#4487=ORIENTED_EDGE('',*,*,#3365,.T.);
#4488=ORIENTED_EDGE('',*,*,#3372,.T.);
#4489=ORIENTED_EDGE('',*,*,#3363,.T.);
#4490=ORIENTED_EDGE('',*,*,#3349,.T.);
#4491=ORIENTED_EDGE('',*,*,#3347,.T.);
#4492=ORIENTED_EDGE('',*,*,#3373,.F.);
#4493=ORIENTED_EDGE('',*,*,#3364,.T.);
#4494=ORIENTED_EDGE('',*,*,#3353,.T.);
#4495=ORIENTED_EDGE('',*,*,#3362,.T.);
#4496=ORIENTED_EDGE('',*,*,#3372,.F.);
#4497=ORIENTED_EDGE('',*,*,#3367,.T.);
#4498=ORIENTED_EDGE('',*,*,#3371,.F.);
#4499=ORIENTED_EDGE('',*,*,#3360,.T.);
#4500=ORIENTED_EDGE('',*,*,#3357,.T.);
#4501=ORIENTED_EDGE('',*,*,#3374,.F.);
#4502=ORIENTED_EDGE('',*,*,#3375,.F.);
#4503=ORIENTED_EDGE('',*,*,#3359,.F.);
#4504=ORIENTED_EDGE('',*,*,#3376,.T.);
#4505=ORIENTED_EDGE('',*,*,#3374,.T.);
#4506=ORIENTED_EDGE('',*,*,#3376,.F.);
#4507=ORIENTED_EDGE('',*,*,#3375,.T.);
#4508=ORIENTED_EDGE('',*,*,#3377,.T.);
#4509=ORIENTED_EDGE('',*,*,#3378,.T.);
#4510=ORIENTED_EDGE('',*,*,#3377,.F.);
#4511=ORIENTED_EDGE('',*,*,#3379,.F.);
#4512=ORIENTED_EDGE('',*,*,#3380,.T.);
#4513=ORIENTED_EDGE('',*,*,#3373,.T.);
#4514=ORIENTED_EDGE('',*,*,#3380,.F.);
#4515=ORIENTED_EDGE('',*,*,#3379,.T.);
#4516=ORIENTED_EDGE('',*,*,#3344,.T.);
#4517=ORIENTED_EDGE('',*,*,#3378,.F.);
#4518=ORIENTED_EDGE('',*,*,#3381,.F.);
#4519=ORIENTED_EDGE('',*,*,#3382,.T.);
#4520=ORIENTED_EDGE('',*,*,#3383,.T.);
#4521=ORIENTED_EDGE('',*,*,#3382,.F.);
#4522=ORIENTED_EDGE('',*,*,#3384,.F.);
#4523=ORIENTED_EDGE('',*,*,#3385,.T.);
#4524=ORIENTED_EDGE('',*,*,#3386,.T.);
#4525=ORIENTED_EDGE('',*,*,#3385,.F.);
#4526=ORIENTED_EDGE('',*,*,#3384,.T.);
#4527=ORIENTED_EDGE('',*,*,#3381,.T.);
#4528=ORIENTED_EDGE('',*,*,#3386,.F.);
#4529=ORIENTED_EDGE('',*,*,#3383,.F.);
#4530=ORIENTED_EDGE('',*,*,#3387,.F.);
#4531=ORIENTED_EDGE('',*,*,#3388,.F.);
#4532=ORIENTED_EDGE('',*,*,#3389,.F.);
#4533=ORIENTED_EDGE('',*,*,#3390,.F.);
#4534=ORIENTED_EDGE('',*,*,#3391,.T.);
#4535=ORIENTED_EDGE('',*,*,#3388,.T.);
#4536=ORIENTED_EDGE('',*,*,#3392,.F.);
#4537=ORIENTED_EDGE('',*,*,#3393,.T.);
#4538=ORIENTED_EDGE('',*,*,#3394,.F.);
#4539=ORIENTED_EDGE('',*,*,#3389,.T.);
#4540=ORIENTED_EDGE('',*,*,#3391,.F.);
#4541=ORIENTED_EDGE('',*,*,#3395,.F.);
#4542=ORIENTED_EDGE('',*,*,#3393,.F.);
#4543=ORIENTED_EDGE('',*,*,#3396,.F.);
#4544=ORIENTED_EDGE('',*,*,#3397,.F.);
#4545=ORIENTED_EDGE('',*,*,#3398,.F.);
#4546=ORIENTED_EDGE('',*,*,#3399,.F.);
#4547=ORIENTED_EDGE('',*,*,#3400,.F.);
#4548=ORIENTED_EDGE('',*,*,#3401,.T.);
#4549=ORIENTED_EDGE('',*,*,#3402,.F.);
#4550=ORIENTED_EDGE('',*,*,#3403,.T.);
#4551=ORIENTED_EDGE('',*,*,#3404,.F.);
#4552=ORIENTED_EDGE('',*,*,#3405,.F.);
#4553=ORIENTED_EDGE('',*,*,#3397,.T.);
#4554=ORIENTED_EDGE('',*,*,#3406,.F.);
#4555=ORIENTED_EDGE('',*,*,#3401,.F.);
#4556=ORIENTED_EDGE('',*,*,#3407,.F.);
#4557=ORIENTED_EDGE('',*,*,#3403,.F.);
#4558=ORIENTED_EDGE('',*,*,#3408,.F.);
#4559=ORIENTED_EDGE('',*,*,#3409,.T.);
#4560=ORIENTED_EDGE('',*,*,#3406,.T.);
#4561=ORIENTED_EDGE('',*,*,#3396,.T.);
#4562=ORIENTED_EDGE('',*,*,#3405,.T.);
#4563=ORIENTED_EDGE('',*,*,#3410,.T.);
#4564=ORIENTED_EDGE('',*,*,#3411,.T.);
#4565=ORIENTED_EDGE('',*,*,#3410,.F.);
#4566=ORIENTED_EDGE('',*,*,#3404,.T.);
#4567=ORIENTED_EDGE('',*,*,#3407,.T.);
#4568=ORIENTED_EDGE('',*,*,#3402,.T.);
#4569=ORIENTED_EDGE('',*,*,#3409,.F.);
#4570=ORIENTED_EDGE('',*,*,#3394,.T.);
#4571=ORIENTED_EDGE('',*,*,#3395,.T.);
#4572=ORIENTED_EDGE('',*,*,#3392,.T.);
#4573=ORIENTED_EDGE('',*,*,#3387,.T.);
#4574=ORIENTED_EDGE('',*,*,#3412,.F.);
#4575=ORIENTED_EDGE('',*,*,#3413,.T.);
#4576=ORIENTED_EDGE('',*,*,#3400,.T.);
#4577=ORIENTED_EDGE('',*,*,#3414,.T.);
#4578=ORIENTED_EDGE('',*,*,#3415,.T.);
#4579=ORIENTED_EDGE('',*,*,#3414,.F.);
#4580=ORIENTED_EDGE('',*,*,#3399,.T.);
#4581=ORIENTED_EDGE('',*,*,#3398,.T.);
#4582=ORIENTED_EDGE('',*,*,#3413,.F.);
#4583=ORIENTED_EDGE('',*,*,#3390,.T.);
#4584=ORIENTED_EDGE('',*,*,#3412,.T.);
#4585=ORIENTED_EDGE('',*,*,#3408,.T.);
#4586=ORIENTED_EDGE('',*,*,#3415,.F.);
#4587=ORIENTED_EDGE('',*,*,#3411,.F.);
#4588=ORIENTED_EDGE('',*,*,#3416,.T.);
#4589=ORIENTED_EDGE('',*,*,#3417,.F.);
#4590=ORIENTED_EDGE('',*,*,#3418,.F.);
#4591=ORIENTED_EDGE('',*,*,#3419,.F.);
#4592=ORIENTED_EDGE('',*,*,#3416,.F.);
#4593=ORIENTED_EDGE('',*,*,#3420,.T.);
#4594=ORIENTED_EDGE('',*,*,#3418,.T.);
#4595=ORIENTED_EDGE('',*,*,#3420,.F.);
#4596=ORIENTED_EDGE('',*,*,#3419,.T.);
#4597=ORIENTED_EDGE('',*,*,#3421,.T.);
#4598=ORIENTED_EDGE('',*,*,#3422,.T.);
#4599=ORIENTED_EDGE('',*,*,#3421,.F.);
#4600=ORIENTED_EDGE('',*,*,#3423,.F.);
#4601=ORIENTED_EDGE('',*,*,#3424,.T.);
#4602=ORIENTED_EDGE('',*,*,#3417,.T.);
#4603=ORIENTED_EDGE('',*,*,#3424,.F.);
#4604=ORIENTED_EDGE('',*,*,#3423,.T.);
#4605=ORIENTED_EDGE('',*,*,#3422,.F.);
#4606=ORIENTED_EDGE('',*,*,#3425,.F.);
#4607=ORIENTED_EDGE('',*,*,#3426,.T.);
#4608=ORIENTED_EDGE('',*,*,#3427,.F.);
#4609=ORIENTED_EDGE('',*,*,#3426,.F.);
#4610=ORIENTED_EDGE('',*,*,#3428,.F.);
#4611=ORIENTED_EDGE('',*,*,#3429,.F.);
#4612=ORIENTED_EDGE('',*,*,#3430,.F.);
#4613=ORIENTED_EDGE('',*,*,#3431,.T.);
#4614=ORIENTED_EDGE('',*,*,#3432,.T.);
#4615=ORIENTED_EDGE('',*,*,#3433,.F.);
#4616=ORIENTED_EDGE('',*,*,#3434,.T.);
#4617=ORIENTED_EDGE('',*,*,#3431,.F.);
#4618=ORIENTED_EDGE('',*,*,#3425,.T.);
#4619=ORIENTED_EDGE('',*,*,#3430,.T.);
#4620=ORIENTED_EDGE('',*,*,#3435,.F.);
#4621=ORIENTED_EDGE('',*,*,#3436,.F.);
#4622=ORIENTED_EDGE('',*,*,#3432,.F.);
#4623=ORIENTED_EDGE('',*,*,#3428,.T.);
#4624=ORIENTED_EDGE('',*,*,#3434,.F.);
#4625=ORIENTED_EDGE('',*,*,#3437,.F.);
#4626=ORIENTED_EDGE('',*,*,#3438,.F.);
#4627=ORIENTED_EDGE('',*,*,#3437,.T.);
#4628=ORIENTED_EDGE('',*,*,#3433,.T.);
#4629=ORIENTED_EDGE('',*,*,#3436,.T.);
#4630=ORIENTED_EDGE('',*,*,#3439,.F.);
#4631=ORIENTED_EDGE('',*,*,#3438,.T.);
#4632=ORIENTED_EDGE('',*,*,#3439,.T.);
#4633=ORIENTED_EDGE('',*,*,#3435,.T.);
#4634=ORIENTED_EDGE('',*,*,#3429,.T.);
#4635=ORIENTED_EDGE('',*,*,#3427,.T.);
#4636=ORIENTED_EDGE('',*,*,#3440,.F.);
#4637=ORIENTED_EDGE('',*,*,#3441,.T.);
#4638=ORIENTED_EDGE('',*,*,#3442,.T.);
#4639=ORIENTED_EDGE('',*,*,#3441,.F.);
#4640=ORIENTED_EDGE('',*,*,#3443,.F.);
#4641=ORIENTED_EDGE('',*,*,#3444,.T.);
#4642=ORIENTED_EDGE('',*,*,#3445,.T.);
#4643=ORIENTED_EDGE('',*,*,#3444,.F.);
#4644=ORIENTED_EDGE('',*,*,#3443,.T.);
#4645=ORIENTED_EDGE('',*,*,#3440,.T.);
#4646=ORIENTED_EDGE('',*,*,#3445,.F.);
#4647=ORIENTED_EDGE('',*,*,#3442,.F.);
#4648=ORIENTED_EDGE('',*,*,#3446,.F.);
#4649=ORIENTED_EDGE('',*,*,#3447,.T.);
#4650=ORIENTED_EDGE('',*,*,#3448,.T.);
#4651=ORIENTED_EDGE('',*,*,#3447,.F.);
#4652=ORIENTED_EDGE('',*,*,#3449,.F.);
#4653=ORIENTED_EDGE('',*,*,#3450,.T.);
#4654=ORIENTED_EDGE('',*,*,#3451,.T.);
#4655=ORIENTED_EDGE('',*,*,#3450,.F.);
#4656=ORIENTED_EDGE('',*,*,#3449,.T.);
#4657=ORIENTED_EDGE('',*,*,#3446,.T.);
#4658=ORIENTED_EDGE('',*,*,#3451,.F.);
#4659=ORIENTED_EDGE('',*,*,#3448,.F.);
#4660=ORIENTED_EDGE('',*,*,#3452,.F.);
#4661=ORIENTED_EDGE('',*,*,#3453,.T.);
#4662=ORIENTED_EDGE('',*,*,#3454,.T.);
#4663=ORIENTED_EDGE('',*,*,#3453,.F.);
#4664=ORIENTED_EDGE('',*,*,#3455,.F.);
#4665=ORIENTED_EDGE('',*,*,#3456,.T.);
#4666=ORIENTED_EDGE('',*,*,#3457,.T.);
#4667=ORIENTED_EDGE('',*,*,#3456,.F.);
#4668=ORIENTED_EDGE('',*,*,#3455,.T.);
#4669=ORIENTED_EDGE('',*,*,#3452,.T.);
#4670=ORIENTED_EDGE('',*,*,#3457,.F.);
#4671=ORIENTED_EDGE('',*,*,#3454,.F.);
#4672=ORIENTED_EDGE('',*,*,#3458,.T.);
#4673=ORIENTED_EDGE('',*,*,#3459,.T.);
#4674=ORIENTED_EDGE('',*,*,#3460,.T.);
#4675=ORIENTED_EDGE('',*,*,#3461,.F.);
#4676=ORIENTED_EDGE('',*,*,#3462,.T.);
#4677=ORIENTED_EDGE('',*,*,#3463,.T.);
#4678=ORIENTED_EDGE('',*,*,#3464,.T.);
#4679=ORIENTED_EDGE('',*,*,#3459,.F.);
#4680=ORIENTED_EDGE('',*,*,#3465,.T.);
#4681=ORIENTED_EDGE('',*,*,#3466,.T.);
#4682=ORIENTED_EDGE('',*,*,#3467,.T.);
#4683=ORIENTED_EDGE('',*,*,#3463,.F.);
#4684=ORIENTED_EDGE('',*,*,#3468,.T.);
#4685=ORIENTED_EDGE('',*,*,#3469,.T.);
#4686=ORIENTED_EDGE('',*,*,#3470,.T.);
#4687=ORIENTED_EDGE('',*,*,#3466,.F.);
#4688=ORIENTED_EDGE('',*,*,#3471,.T.);
#4689=ORIENTED_EDGE('',*,*,#3472,.T.);
#4690=ORIENTED_EDGE('',*,*,#3473,.T.);
#4691=ORIENTED_EDGE('',*,*,#3469,.F.);
#4692=ORIENTED_EDGE('',*,*,#3474,.T.);
#4693=ORIENTED_EDGE('',*,*,#3461,.T.);
#4694=ORIENTED_EDGE('',*,*,#3475,.T.);
#4695=ORIENTED_EDGE('',*,*,#3472,.F.);
#4696=ORIENTED_EDGE('',*,*,#3474,.F.);
#4697=ORIENTED_EDGE('',*,*,#3471,.F.);
#4698=ORIENTED_EDGE('',*,*,#3468,.F.);
#4699=ORIENTED_EDGE('',*,*,#3465,.F.);
#4700=ORIENTED_EDGE('',*,*,#3462,.F.);
#4701=ORIENTED_EDGE('',*,*,#3458,.F.);
#4702=ORIENTED_EDGE('',*,*,#3475,.F.);
#4703=ORIENTED_EDGE('',*,*,#3460,.F.);
#4704=ORIENTED_EDGE('',*,*,#3464,.F.);
#4705=ORIENTED_EDGE('',*,*,#3467,.F.);
#4706=ORIENTED_EDGE('',*,*,#3470,.F.);
#4707=ORIENTED_EDGE('',*,*,#3473,.F.);
#4708=ORIENTED_EDGE('',*,*,#3476,.F.);
#4709=ORIENTED_EDGE('',*,*,#3477,.F.);
#4710=ORIENTED_EDGE('',*,*,#3478,.F.);
#4711=ORIENTED_EDGE('',*,*,#3479,.T.);
#4712=ORIENTED_EDGE('',*,*,#3477,.T.);
#4713=ORIENTED_EDGE('',*,*,#3479,.F.);
#4714=ORIENTED_EDGE('',*,*,#3480,.F.);
#4715=ORIENTED_EDGE('',*,*,#3481,.T.);
#4716=ORIENTED_EDGE('',*,*,#3478,.T.);
#4717=ORIENTED_EDGE('',*,*,#3481,.F.);
#4718=ORIENTED_EDGE('',*,*,#3482,.F.);
#4719=ORIENTED_EDGE('',*,*,#3483,.T.);
#4720=ORIENTED_EDGE('',*,*,#3480,.T.);
#4721=ORIENTED_EDGE('',*,*,#3483,.F.);
#4722=ORIENTED_EDGE('',*,*,#3482,.T.);
#4723=ORIENTED_EDGE('',*,*,#3484,.F.);
#4724=ORIENTED_EDGE('',*,*,#3485,.F.);
#4725=ORIENTED_EDGE('',*,*,#3486,.T.);
#4726=ORIENTED_EDGE('',*,*,#3484,.T.);
#4727=ORIENTED_EDGE('',*,*,#3486,.F.);
#4728=ORIENTED_EDGE('',*,*,#3476,.T.);
#4729=ORIENTED_EDGE('',*,*,#3487,.T.);
#4730=ORIENTED_EDGE('',*,*,#3485,.T.);
#4731=ORIENTED_EDGE('',*,*,#3487,.F.);
#4732=ORIENTED_EDGE('',*,*,#3488,.F.);
#4733=ORIENTED_EDGE('',*,*,#3489,.T.);
#4734=ORIENTED_EDGE('',*,*,#3490,.F.);
#4735=ORIENTED_EDGE('',*,*,#3489,.F.);
#4736=ORIENTED_EDGE('',*,*,#3491,.F.);
#4737=ORIENTED_EDGE('',*,*,#3492,.T.);
#4738=ORIENTED_EDGE('',*,*,#3493,.F.);
#4739=ORIENTED_EDGE('',*,*,#3492,.F.);
#4740=ORIENTED_EDGE('',*,*,#3494,.F.);
#4741=ORIENTED_EDGE('',*,*,#3495,.T.);
#4742=ORIENTED_EDGE('',*,*,#3496,.F.);
#4743=ORIENTED_EDGE('',*,*,#3495,.F.);
#4744=ORIENTED_EDGE('',*,*,#3497,.F.);
#4745=ORIENTED_EDGE('',*,*,#3498,.T.);
#4746=ORIENTED_EDGE('',*,*,#3499,.F.);
#4747=ORIENTED_EDGE('',*,*,#3498,.F.);
#4748=ORIENTED_EDGE('',*,*,#3500,.F.);
#4749=ORIENTED_EDGE('',*,*,#3501,.F.);
#4750=ORIENTED_EDGE('',*,*,#3502,.F.);
#4751=ORIENTED_EDGE('',*,*,#3503,.F.);
#4752=ORIENTED_EDGE('',*,*,#3504,.F.);
#4753=ORIENTED_EDGE('',*,*,#3505,.F.);
#4754=ORIENTED_EDGE('',*,*,#3506,.F.);
#4755=ORIENTED_EDGE('',*,*,#3507,.F.);
#4756=ORIENTED_EDGE('',*,*,#3508,.F.);
#4757=ORIENTED_EDGE('',*,*,#3509,.F.);
#4758=ORIENTED_EDGE('',*,*,#3510,.F.);
#4759=ORIENTED_EDGE('',*,*,#3511,.F.);
#4760=ORIENTED_EDGE('',*,*,#3512,.F.);
#4761=ORIENTED_EDGE('',*,*,#3513,.F.);
#4762=ORIENTED_EDGE('',*,*,#3514,.F.);
#4763=ORIENTED_EDGE('',*,*,#3515,.F.);
#4764=ORIENTED_EDGE('',*,*,#3501,.T.);
#4765=ORIENTED_EDGE('',*,*,#3516,.T.);
#4766=ORIENTED_EDGE('',*,*,#3517,.T.);
#4767=ORIENTED_EDGE('',*,*,#3518,.F.);
#4768=ORIENTED_EDGE('',*,*,#3505,.T.);
#4769=ORIENTED_EDGE('',*,*,#3519,.T.);
#4770=ORIENTED_EDGE('',*,*,#3520,.T.);
#4771=ORIENTED_EDGE('',*,*,#3521,.F.);
#4772=ORIENTED_EDGE('',*,*,#3509,.T.);
#4773=ORIENTED_EDGE('',*,*,#3522,.T.);
#4774=ORIENTED_EDGE('',*,*,#3523,.T.);
#4775=ORIENTED_EDGE('',*,*,#3524,.F.);
#4776=ORIENTED_EDGE('',*,*,#3502,.T.);
#4777=ORIENTED_EDGE('',*,*,#3518,.T.);
#4778=ORIENTED_EDGE('',*,*,#3525,.T.);
#4779=ORIENTED_EDGE('',*,*,#3526,.T.);
#4780=ORIENTED_EDGE('',*,*,#3527,.T.);
#4781=ORIENTED_EDGE('',*,*,#3528,.T.);
#4782=ORIENTED_EDGE('',*,*,#3529,.T.);
#4783=ORIENTED_EDGE('',*,*,#3530,.T.);
#4784=ORIENTED_EDGE('',*,*,#3531,.T.);
#4785=ORIENTED_EDGE('',*,*,#3532,.T.);
#4786=ORIENTED_EDGE('',*,*,#3513,.T.);
#4787=ORIENTED_EDGE('',*,*,#3533,.T.);
#4788=ORIENTED_EDGE('',*,*,#3534,.T.);
#4789=ORIENTED_EDGE('',*,*,#3535,.T.);
#4790=ORIENTED_EDGE('',*,*,#3536,.T.);
#4791=ORIENTED_EDGE('',*,*,#3537,.T.);
#4792=ORIENTED_EDGE('',*,*,#3538,.T.);
#4793=ORIENTED_EDGE('',*,*,#3539,.T.);
#4794=ORIENTED_EDGE('',*,*,#3540,.T.);
#4795=ORIENTED_EDGE('',*,*,#3541,.T.);
#4796=ORIENTED_EDGE('',*,*,#3510,.T.);
#4797=ORIENTED_EDGE('',*,*,#3524,.T.);
#4798=ORIENTED_EDGE('',*,*,#3542,.T.);
#4799=ORIENTED_EDGE('',*,*,#3543,.T.);
#4800=ORIENTED_EDGE('',*,*,#3544,.T.);
#4801=ORIENTED_EDGE('',*,*,#3545,.T.);
#4802=ORIENTED_EDGE('',*,*,#3546,.T.);
#4803=ORIENTED_EDGE('',*,*,#3547,.T.);
#4804=ORIENTED_EDGE('',*,*,#3548,.T.);
#4805=ORIENTED_EDGE('',*,*,#3549,.T.);
#4806=ORIENTED_EDGE('',*,*,#3506,.T.);
#4807=ORIENTED_EDGE('',*,*,#3521,.T.);
#4808=ORIENTED_EDGE('',*,*,#3550,.T.);
#4809=ORIENTED_EDGE('',*,*,#3551,.T.);
#4810=ORIENTED_EDGE('',*,*,#3552,.T.);
#4811=ORIENTED_EDGE('',*,*,#3553,.T.);
#4812=ORIENTED_EDGE('',*,*,#3554,.T.);
#4813=ORIENTED_EDGE('',*,*,#3555,.T.);
#4814=ORIENTED_EDGE('',*,*,#3556,.T.);
#4815=ORIENTED_EDGE('',*,*,#3557,.T.);
#4816=ORIENTED_EDGE('',*,*,#3490,.T.);
#4817=ORIENTED_EDGE('',*,*,#3493,.T.);
#4818=ORIENTED_EDGE('',*,*,#3496,.T.);
#4819=ORIENTED_EDGE('',*,*,#3499,.T.);
#4820=ORIENTED_EDGE('',*,*,#3512,.T.);
#4821=ORIENTED_EDGE('',*,*,#3558,.T.);
#4822=ORIENTED_EDGE('',*,*,#3559,.T.);
#4823=ORIENTED_EDGE('',*,*,#3533,.F.);
#4824=ORIENTED_EDGE('',*,*,#3514,.T.);
#4825=ORIENTED_EDGE('',*,*,#3532,.F.);
#4826=ORIENTED_EDGE('',*,*,#3560,.T.);
#4827=ORIENTED_EDGE('',*,*,#3561,.T.);
#4828=ORIENTED_EDGE('',*,*,#3531,.F.);
#4829=ORIENTED_EDGE('',*,*,#3562,.F.);
#4830=ORIENTED_EDGE('',*,*,#3563,.F.);
#4831=ORIENTED_EDGE('',*,*,#3560,.F.);
#4832=ORIENTED_EDGE('',*,*,#3530,.F.);
#4833=ORIENTED_EDGE('',*,*,#3564,.F.);
#4834=ORIENTED_EDGE('',*,*,#3565,.F.);
#4835=ORIENTED_EDGE('',*,*,#3562,.T.);
#4836=ORIENTED_EDGE('',*,*,#3526,.F.);
#4837=ORIENTED_EDGE('',*,*,#3566,.F.);
#4838=ORIENTED_EDGE('',*,*,#3567,.F.);
#4839=ORIENTED_EDGE('',*,*,#3568,.F.);
#4840=ORIENTED_EDGE('',*,*,#3525,.F.);
#4841=ORIENTED_EDGE('',*,*,#3517,.F.);
#4842=ORIENTED_EDGE('',*,*,#3569,.F.);
#4843=ORIENTED_EDGE('',*,*,#3566,.T.);
#4844=ORIENTED_EDGE('',*,*,#3568,.T.);
#4845=ORIENTED_EDGE('',*,*,#3570,.F.);
#4846=ORIENTED_EDGE('',*,*,#3571,.T.);
#4847=ORIENTED_EDGE('',*,*,#3527,.F.);
#4848=ORIENTED_EDGE('',*,*,#3500,.T.);
#4849=ORIENTED_EDGE('',*,*,#3572,.F.);
#4850=ORIENTED_EDGE('',*,*,#3573,.T.);
#4851=ORIENTED_EDGE('',*,*,#3574,.T.);
#4852=ORIENTED_EDGE('',*,*,#3575,.T.);
#4853=ORIENTED_EDGE('',*,*,#3576,.T.);
#4854=ORIENTED_EDGE('',*,*,#3577,.T.);
#4855=ORIENTED_EDGE('',*,*,#3578,.T.);
#4856=ORIENTED_EDGE('',*,*,#3570,.T.);
#4857=ORIENTED_EDGE('',*,*,#3567,.T.);
#4858=ORIENTED_EDGE('',*,*,#3569,.T.);
#4859=ORIENTED_EDGE('',*,*,#3516,.F.);
#4860=ORIENTED_EDGE('',*,*,#3488,.T.);
#4861=ORIENTED_EDGE('',*,*,#3515,.T.);
#4862=ORIENTED_EDGE('',*,*,#3561,.F.);
#4863=ORIENTED_EDGE('',*,*,#3563,.T.);
#4864=ORIENTED_EDGE('',*,*,#3565,.T.);
#4865=ORIENTED_EDGE('',*,*,#3579,.T.);
#4866=ORIENTED_EDGE('',*,*,#3580,.T.);
#4867=ORIENTED_EDGE('',*,*,#3581,.T.);
#4868=ORIENTED_EDGE('',*,*,#3582,.T.);
#4869=ORIENTED_EDGE('',*,*,#3583,.T.);
#4870=ORIENTED_EDGE('',*,*,#3584,.T.);
#4871=ORIENTED_EDGE('',*,*,#3585,.T.);
#4872=ORIENTED_EDGE('',*,*,#3558,.F.);
#4873=ORIENTED_EDGE('',*,*,#3497,.T.);
#4874=ORIENTED_EDGE('',*,*,#3586,.F.);
#4875=ORIENTED_EDGE('',*,*,#3587,.T.);
#4876=ORIENTED_EDGE('',*,*,#3588,.F.);
#4877=ORIENTED_EDGE('',*,*,#3580,.F.);
#4878=ORIENTED_EDGE('',*,*,#3589,.T.);
#4879=ORIENTED_EDGE('',*,*,#3528,.F.);
#4880=ORIENTED_EDGE('',*,*,#3571,.F.);
#4881=ORIENTED_EDGE('',*,*,#3578,.F.);
#4882=ORIENTED_EDGE('',*,*,#3590,.F.);
#4883=ORIENTED_EDGE('',*,*,#3587,.F.);
#4884=ORIENTED_EDGE('',*,*,#3588,.T.);
#4885=ORIENTED_EDGE('',*,*,#3586,.T.);
#4886=ORIENTED_EDGE('',*,*,#3590,.T.);
#4887=ORIENTED_EDGE('',*,*,#3577,.F.);
#4888=ORIENTED_EDGE('',*,*,#3591,.T.);
#4889=ORIENTED_EDGE('',*,*,#3592,.T.);
#4890=ORIENTED_EDGE('',*,*,#3593,.T.);
#4891=ORIENTED_EDGE('',*,*,#3594,.T.);
#4892=ORIENTED_EDGE('',*,*,#3593,.F.);
#4893=ORIENTED_EDGE('',*,*,#3595,.T.);
#4894=ORIENTED_EDGE('',*,*,#3596,.T.);
#4895=ORIENTED_EDGE('',*,*,#3597,.F.);
#4896=ORIENTED_EDGE('',*,*,#3598,.T.);
#4897=ORIENTED_EDGE('',*,*,#3599,.T.);
#4898=ORIENTED_EDGE('',*,*,#3600,.T.);
#4899=ORIENTED_EDGE('',*,*,#3601,.F.);
#4900=ORIENTED_EDGE('',*,*,#3602,.T.);
#4901=ORIENTED_EDGE('',*,*,#3603,.T.);
#4902=ORIENTED_EDGE('',*,*,#3604,.T.);
#4903=ORIENTED_EDGE('',*,*,#3581,.F.);
#4904=ORIENTED_EDGE('',*,*,#3564,.T.);
#4905=ORIENTED_EDGE('',*,*,#3529,.F.);
#4906=ORIENTED_EDGE('',*,*,#3589,.F.);
#4907=ORIENTED_EDGE('',*,*,#3579,.F.);
#4908=ORIENTED_EDGE('',*,*,#3503,.T.);
#4909=ORIENTED_EDGE('',*,*,#3557,.F.);
#4910=ORIENTED_EDGE('',*,*,#3605,.T.);
#4911=ORIENTED_EDGE('',*,*,#3572,.T.);
#4912=ORIENTED_EDGE('',*,*,#3556,.F.);
#4913=ORIENTED_EDGE('',*,*,#3606,.F.);
#4914=ORIENTED_EDGE('',*,*,#3573,.F.);
#4915=ORIENTED_EDGE('',*,*,#3605,.F.);
#4916=ORIENTED_EDGE('',*,*,#3555,.F.);
#4917=ORIENTED_EDGE('',*,*,#3607,.F.);
#4918=ORIENTED_EDGE('',*,*,#3574,.F.);
#4919=ORIENTED_EDGE('',*,*,#3606,.T.);
#4920=ORIENTED_EDGE('',*,*,#3551,.F.);
#4921=ORIENTED_EDGE('',*,*,#3608,.F.);
#4922=ORIENTED_EDGE('',*,*,#3609,.F.);
#4923=ORIENTED_EDGE('',*,*,#3610,.F.);
#4924=ORIENTED_EDGE('',*,*,#3550,.F.);
#4925=ORIENTED_EDGE('',*,*,#3520,.F.);
#4926=ORIENTED_EDGE('',*,*,#3611,.F.);
#4927=ORIENTED_EDGE('',*,*,#3608,.T.);
#4928=ORIENTED_EDGE('',*,*,#3610,.T.);
#4929=ORIENTED_EDGE('',*,*,#3612,.F.);
#4930=ORIENTED_EDGE('',*,*,#3613,.T.);
#4931=ORIENTED_EDGE('',*,*,#3552,.F.);
#4932=ORIENTED_EDGE('',*,*,#3504,.T.);
#4933=ORIENTED_EDGE('',*,*,#3614,.F.);
#4934=ORIENTED_EDGE('',*,*,#3615,.T.);
#4935=ORIENTED_EDGE('',*,*,#3616,.T.);
#4936=ORIENTED_EDGE('',*,*,#3617,.T.);
#4937=ORIENTED_EDGE('',*,*,#3618,.T.);
#4938=ORIENTED_EDGE('',*,*,#3597,.T.);
#4939=ORIENTED_EDGE('',*,*,#3619,.T.);
#4940=ORIENTED_EDGE('',*,*,#3612,.T.);
#4941=ORIENTED_EDGE('',*,*,#3609,.T.);
#4942=ORIENTED_EDGE('',*,*,#3611,.T.);
#4943=ORIENTED_EDGE('',*,*,#3519,.F.);
#4944=ORIENTED_EDGE('',*,*,#3491,.T.);
#4945=ORIENTED_EDGE('',*,*,#3592,.F.);
#4946=ORIENTED_EDGE('',*,*,#3620,.T.);
#4947=ORIENTED_EDGE('',*,*,#3595,.F.);
#4948=ORIENTED_EDGE('',*,*,#3591,.F.);
#4949=ORIENTED_EDGE('',*,*,#3576,.F.);
#4950=ORIENTED_EDGE('',*,*,#3621,.T.);
#4951=ORIENTED_EDGE('',*,*,#3553,.F.);
#4952=ORIENTED_EDGE('',*,*,#3613,.F.);
#4953=ORIENTED_EDGE('',*,*,#3619,.F.);
#4954=ORIENTED_EDGE('',*,*,#3596,.F.);
#4955=ORIENTED_EDGE('',*,*,#3620,.F.);
#4956=ORIENTED_EDGE('',*,*,#3607,.T.);
#4957=ORIENTED_EDGE('',*,*,#3554,.F.);
#4958=ORIENTED_EDGE('',*,*,#3621,.F.);
#4959=ORIENTED_EDGE('',*,*,#3575,.F.);
#4960=ORIENTED_EDGE('',*,*,#3507,.T.);
#4961=ORIENTED_EDGE('',*,*,#3549,.F.);
#4962=ORIENTED_EDGE('',*,*,#3622,.T.);
#4963=ORIENTED_EDGE('',*,*,#3614,.T.);
#4964=ORIENTED_EDGE('',*,*,#3548,.F.);
#4965=ORIENTED_EDGE('',*,*,#3623,.F.);
#4966=ORIENTED_EDGE('',*,*,#3615,.F.);
#4967=ORIENTED_EDGE('',*,*,#3622,.F.);
#4968=ORIENTED_EDGE('',*,*,#3547,.F.);
#4969=ORIENTED_EDGE('',*,*,#3624,.F.);
#4970=ORIENTED_EDGE('',*,*,#3616,.F.);
#4971=ORIENTED_EDGE('',*,*,#3623,.T.);
#4972=ORIENTED_EDGE('',*,*,#3543,.F.);
#4973=ORIENTED_EDGE('',*,*,#3625,.F.);
#4974=ORIENTED_EDGE('',*,*,#3626,.F.);
#4975=ORIENTED_EDGE('',*,*,#3627,.F.);
#4976=ORIENTED_EDGE('',*,*,#3542,.F.);
#4977=ORIENTED_EDGE('',*,*,#3523,.F.);
#4978=ORIENTED_EDGE('',*,*,#3628,.F.);
#4979=ORIENTED_EDGE('',*,*,#3625,.T.);
#4980=ORIENTED_EDGE('',*,*,#3627,.T.);
#4981=ORIENTED_EDGE('',*,*,#3629,.F.);
#4982=ORIENTED_EDGE('',*,*,#3630,.T.);
#4983=ORIENTED_EDGE('',*,*,#3544,.F.);
#4984=ORIENTED_EDGE('',*,*,#3508,.T.);
#4985=ORIENTED_EDGE('',*,*,#3631,.F.);
#4986=ORIENTED_EDGE('',*,*,#3632,.T.);
#4987=ORIENTED_EDGE('',*,*,#3633,.T.);
#4988=ORIENTED_EDGE('',*,*,#3634,.T.);
#4989=ORIENTED_EDGE('',*,*,#3635,.T.);
#4990=ORIENTED_EDGE('',*,*,#3601,.T.);
#4991=ORIENTED_EDGE('',*,*,#3636,.T.);
#4992=ORIENTED_EDGE('',*,*,#3629,.T.);
#4993=ORIENTED_EDGE('',*,*,#3626,.T.);
#4994=ORIENTED_EDGE('',*,*,#3628,.T.);
#4995=ORIENTED_EDGE('',*,*,#3522,.F.);
#4996=ORIENTED_EDGE('',*,*,#3494,.T.);
#4997=ORIENTED_EDGE('',*,*,#3599,.F.);
#4998=ORIENTED_EDGE('',*,*,#3637,.T.);
#4999=ORIENTED_EDGE('',*,*,#3598,.F.);
#5000=ORIENTED_EDGE('',*,*,#3618,.F.);
#5001=ORIENTED_EDGE('',*,*,#3638,.T.);
#5002=ORIENTED_EDGE('',*,*,#3545,.F.);
#5003=ORIENTED_EDGE('',*,*,#3630,.F.);
#5004=ORIENTED_EDGE('',*,*,#3636,.F.);
#5005=ORIENTED_EDGE('',*,*,#3600,.F.);
#5006=ORIENTED_EDGE('',*,*,#3637,.F.);
#5007=ORIENTED_EDGE('',*,*,#3624,.T.);
#5008=ORIENTED_EDGE('',*,*,#3546,.F.);
#5009=ORIENTED_EDGE('',*,*,#3638,.F.);
#5010=ORIENTED_EDGE('',*,*,#3617,.F.);
#5011=ORIENTED_EDGE('',*,*,#3511,.T.);
#5012=ORIENTED_EDGE('',*,*,#3541,.F.);
#5013=ORIENTED_EDGE('',*,*,#3639,.T.);
#5014=ORIENTED_EDGE('',*,*,#3631,.T.);
#5015=ORIENTED_EDGE('',*,*,#3540,.F.);
#5016=ORIENTED_EDGE('',*,*,#3640,.F.);
#5017=ORIENTED_EDGE('',*,*,#3632,.F.);
#5018=ORIENTED_EDGE('',*,*,#3639,.F.);
#5019=ORIENTED_EDGE('',*,*,#3585,.F.);
#5020=ORIENTED_EDGE('',*,*,#3641,.T.);
#5021=ORIENTED_EDGE('',*,*,#3534,.F.);
#5022=ORIENTED_EDGE('',*,*,#3559,.F.);
#5023=ORIENTED_EDGE('',*,*,#3584,.F.);
#5024=ORIENTED_EDGE('',*,*,#3642,.F.);
#5025=ORIENTED_EDGE('',*,*,#3535,.F.);
#5026=ORIENTED_EDGE('',*,*,#3641,.F.);
#5027=ORIENTED_EDGE('',*,*,#3539,.F.);
#5028=ORIENTED_EDGE('',*,*,#3643,.F.);
#5029=ORIENTED_EDGE('',*,*,#3633,.F.);
#5030=ORIENTED_EDGE('',*,*,#3640,.T.);
#5031=ORIENTED_EDGE('',*,*,#3603,.F.);
#5032=ORIENTED_EDGE('',*,*,#3644,.T.);
#5033=ORIENTED_EDGE('',*,*,#3602,.F.);
#5034=ORIENTED_EDGE('',*,*,#3635,.F.);
#5035=ORIENTED_EDGE('',*,*,#3645,.T.);
#5036=ORIENTED_EDGE('',*,*,#3537,.F.);
#5037=ORIENTED_EDGE('',*,*,#3646,.F.);
#5038=ORIENTED_EDGE('',*,*,#3582,.F.);
#5039=ORIENTED_EDGE('',*,*,#3604,.F.);
#5040=ORIENTED_EDGE('',*,*,#3644,.F.);
#5041=ORIENTED_EDGE('',*,*,#3643,.T.);
#5042=ORIENTED_EDGE('',*,*,#3538,.F.);
#5043=ORIENTED_EDGE('',*,*,#3645,.F.);
#5044=ORIENTED_EDGE('',*,*,#3634,.F.);
#5045=ORIENTED_EDGE('',*,*,#3642,.T.);
#5046=ORIENTED_EDGE('',*,*,#3583,.F.);
#5047=ORIENTED_EDGE('',*,*,#3646,.T.);
#5048=ORIENTED_EDGE('',*,*,#3536,.F.);
#5049=ORIENTED_EDGE('',*,*,#3594,.F.);
#5050=ORIENTED_EDGE('',*,*,#3647,.F.);
#5051=ORIENTED_EDGE('',*,*,#3647,.T.);
#5052=ORIENTED_EDGE('',*,*,#3648,.T.);
#5053=ORIENTED_EDGE('',*,*,#3649,.T.);
#5054=ORIENTED_EDGE('',*,*,#3648,.F.);
#5055=ORIENTED_EDGE('',*,*,#3649,.F.);
#5056=ORIENTED_EDGE('',*,*,#3650,.F.);
#5057=ORIENTED_EDGE('',*,*,#3651,.T.);
#5058=ORIENTED_EDGE('',*,*,#3652,.T.);
#5059=ORIENTED_EDGE('',*,*,#3651,.F.);
#5060=ORIENTED_EDGE('',*,*,#3653,.F.);
#5061=ORIENTED_EDGE('',*,*,#3654,.T.);
#5062=ORIENTED_EDGE('',*,*,#3655,.T.);
#5063=ORIENTED_EDGE('',*,*,#3654,.F.);
#5064=ORIENTED_EDGE('',*,*,#3653,.T.);
#5065=ORIENTED_EDGE('',*,*,#3650,.T.);
#5066=ORIENTED_EDGE('',*,*,#3655,.F.);
#5067=ORIENTED_EDGE('',*,*,#3652,.F.);
#5068=ORIENTED_EDGE('',*,*,#3656,.F.);
#5069=ORIENTED_EDGE('',*,*,#3657,.F.);
#5070=ORIENTED_EDGE('',*,*,#3658,.F.);
#5071=ORIENTED_EDGE('',*,*,#3659,.F.);
#5072=ORIENTED_EDGE('',*,*,#3660,.T.);
#5073=ORIENTED_EDGE('',*,*,#3657,.T.);
#5074=ORIENTED_EDGE('',*,*,#3661,.F.);
#5075=ORIENTED_EDGE('',*,*,#3662,.T.);
#5076=ORIENTED_EDGE('',*,*,#3663,.F.);
#5077=ORIENTED_EDGE('',*,*,#3658,.T.);
#5078=ORIENTED_EDGE('',*,*,#3660,.F.);
#5079=ORIENTED_EDGE('',*,*,#3664,.F.);
#5080=ORIENTED_EDGE('',*,*,#3662,.F.);
#5081=ORIENTED_EDGE('',*,*,#3665,.F.);
#5082=ORIENTED_EDGE('',*,*,#3666,.F.);
#5083=ORIENTED_EDGE('',*,*,#3667,.F.);
#5084=ORIENTED_EDGE('',*,*,#3668,.F.);
#5085=ORIENTED_EDGE('',*,*,#3669,.F.);
#5086=ORIENTED_EDGE('',*,*,#3670,.T.);
#5087=ORIENTED_EDGE('',*,*,#3671,.F.);
#5088=ORIENTED_EDGE('',*,*,#3672,.T.);
#5089=ORIENTED_EDGE('',*,*,#3673,.F.);
#5090=ORIENTED_EDGE('',*,*,#3674,.F.);
#5091=ORIENTED_EDGE('',*,*,#3666,.T.);
#5092=ORIENTED_EDGE('',*,*,#3675,.F.);
#5093=ORIENTED_EDGE('',*,*,#3670,.F.);
#5094=ORIENTED_EDGE('',*,*,#3676,.F.);
#5095=ORIENTED_EDGE('',*,*,#3672,.F.);
#5096=ORIENTED_EDGE('',*,*,#3677,.F.);
#5097=ORIENTED_EDGE('',*,*,#3678,.T.);
#5098=ORIENTED_EDGE('',*,*,#3675,.T.);
#5099=ORIENTED_EDGE('',*,*,#3665,.T.);
#5100=ORIENTED_EDGE('',*,*,#3674,.T.);
#5101=ORIENTED_EDGE('',*,*,#3679,.T.);
#5102=ORIENTED_EDGE('',*,*,#3680,.T.);
#5103=ORIENTED_EDGE('',*,*,#3679,.F.);
#5104=ORIENTED_EDGE('',*,*,#3673,.T.);
#5105=ORIENTED_EDGE('',*,*,#3676,.T.);
#5106=ORIENTED_EDGE('',*,*,#3671,.T.);
#5107=ORIENTED_EDGE('',*,*,#3678,.F.);
#5108=ORIENTED_EDGE('',*,*,#3663,.T.);
#5109=ORIENTED_EDGE('',*,*,#3664,.T.);
#5110=ORIENTED_EDGE('',*,*,#3661,.T.);
#5111=ORIENTED_EDGE('',*,*,#3656,.T.);
#5112=ORIENTED_EDGE('',*,*,#3681,.F.);
#5113=ORIENTED_EDGE('',*,*,#3682,.T.);
#5114=ORIENTED_EDGE('',*,*,#3669,.T.);
#5115=ORIENTED_EDGE('',*,*,#3683,.T.);
#5116=ORIENTED_EDGE('',*,*,#3684,.T.);
#5117=ORIENTED_EDGE('',*,*,#3683,.F.);
#5118=ORIENTED_EDGE('',*,*,#3668,.T.);
#5119=ORIENTED_EDGE('',*,*,#3667,.T.);
#5120=ORIENTED_EDGE('',*,*,#3682,.F.);
#5121=ORIENTED_EDGE('',*,*,#3659,.T.);
#5122=ORIENTED_EDGE('',*,*,#3681,.T.);
#5123=ORIENTED_EDGE('',*,*,#3677,.T.);
#5124=ORIENTED_EDGE('',*,*,#3684,.F.);
#5125=ORIENTED_EDGE('',*,*,#3680,.F.);
#5126=ORIENTED_EDGE('',*,*,#3685,.F.);
#5127=ORIENTED_EDGE('',*,*,#3686,.F.);
#5128=ORIENTED_EDGE('',*,*,#3687,.T.);
#5129=ORIENTED_EDGE('',*,*,#3688,.T.);
#5130=ORIENTED_EDGE('',*,*,#3689,.F.);
#5131=ORIENTED_EDGE('',*,*,#3690,.F.);
#5132=ORIENTED_EDGE('',*,*,#3691,.T.);
#5133=ORIENTED_EDGE('',*,*,#3692,.T.);
#5134=ORIENTED_EDGE('',*,*,#3687,.F.);
#5135=ORIENTED_EDGE('',*,*,#3693,.F.);
#5136=ORIENTED_EDGE('',*,*,#3694,.T.);
#5137=ORIENTED_EDGE('',*,*,#3695,.T.);
#5138=ORIENTED_EDGE('',*,*,#3691,.F.);
#5139=ORIENTED_EDGE('',*,*,#3696,.F.);
#5140=ORIENTED_EDGE('',*,*,#3697,.T.);
#5141=ORIENTED_EDGE('',*,*,#3698,.T.);
#5142=ORIENTED_EDGE('',*,*,#3694,.F.);
#5143=ORIENTED_EDGE('',*,*,#3699,.F.);
#5144=ORIENTED_EDGE('',*,*,#3700,.T.);
#5145=ORIENTED_EDGE('',*,*,#3701,.T.);
#5146=ORIENTED_EDGE('',*,*,#3697,.F.);
#5147=ORIENTED_EDGE('',*,*,#3702,.F.);
#5148=ORIENTED_EDGE('',*,*,#3689,.T.);
#5149=ORIENTED_EDGE('',*,*,#3703,.T.);
#5150=ORIENTED_EDGE('',*,*,#3700,.F.);
#5151=ORIENTED_EDGE('',*,*,#3703,.F.);
#5152=ORIENTED_EDGE('',*,*,#3688,.F.);
#5153=ORIENTED_EDGE('',*,*,#3692,.F.);
#5154=ORIENTED_EDGE('',*,*,#3695,.F.);
#5155=ORIENTED_EDGE('',*,*,#3698,.F.);
#5156=ORIENTED_EDGE('',*,*,#3701,.F.);
#5157=ORIENTED_EDGE('',*,*,#3704,.F.);
#5158=ORIENTED_EDGE('',*,*,#3686,.T.);
#5159=ORIENTED_EDGE('',*,*,#3702,.T.);
#5160=ORIENTED_EDGE('',*,*,#3699,.T.);
#5161=ORIENTED_EDGE('',*,*,#3696,.T.);
#5162=ORIENTED_EDGE('',*,*,#3693,.T.);
#5163=ORIENTED_EDGE('',*,*,#3690,.T.);
#5164=ORIENTED_EDGE('',*,*,#3705,.F.);
#5165=ORIENTED_EDGE('',*,*,#3706,.T.);
#5166=ORIENTED_EDGE('',*,*,#3704,.T.);
#5167=ORIENTED_EDGE('',*,*,#3706,.F.);
#5168=ORIENTED_EDGE('',*,*,#3685,.T.);
#5169=ORIENTED_EDGE('',*,*,#3707,.T.);
#5170=ORIENTED_EDGE('',*,*,#3705,.T.);
#5171=ORIENTED_EDGE('',*,*,#3707,.F.);
#5172=CYLINDRICAL_SURFACE('',#5931,0.165);
#5173=CYLINDRICAL_SURFACE('',#5935,0.165);
#5174=CYLINDRICAL_SURFACE('',#5939,0.165);
#5175=CYLINDRICAL_SURFACE('',#5943,0.165);
#5176=CYLINDRICAL_SURFACE('',#5947,1.5);
#5177=CYLINDRICAL_SURFACE('',#5952,1.02);
#5178=CYLINDRICAL_SURFACE('',#5954,0.165);
#5179=CYLINDRICAL_SURFACE('',#5958,0.165);
#5180=CYLINDRICAL_SURFACE('',#5962,0.165);
#5181=CYLINDRICAL_SURFACE('',#5966,0.165);
#5182=CYLINDRICAL_SURFACE('',#5970,1.5);
#5183=CYLINDRICAL_SURFACE('',#5975,1.02);
#5184=CYLINDRICAL_SURFACE('',#5977,0.5);
#5185=CYLINDRICAL_SURFACE('',#5982,0.5);
#5186=CYLINDRICAL_SURFACE('',#5987,0.5);
#5187=CYLINDRICAL_SURFACE('',#5992,0.5);
#5188=CYLINDRICAL_SURFACE('',#5997,0.275);
#5189=CYLINDRICAL_SURFACE('',#5999,0.275);
#5190=CYLINDRICAL_SURFACE('',#6001,0.275);
#5191=CYLINDRICAL_SURFACE('',#6003,0.275);
#5192=CYLINDRICAL_SURFACE('',#6018,0.25);
#5193=CYLINDRICAL_SURFACE('',#6020,0.25);
#5194=CYLINDRICAL_SURFACE('',#6024,0.33);
#5195=CYLINDRICAL_SURFACE('',#6027,0.33);
#5196=CYLINDRICAL_SURFACE('',#6030,0.33);
#5197=CYLINDRICAL_SURFACE('',#6033,0.33);
#5198=CYLINDRICAL_SURFACE('',#6040,0.21);
#5199=CYLINDRICAL_SURFACE('',#6042,0.21);
#5200=CYLINDRICAL_SURFACE('',#6044,0.21);
#5201=CYLINDRICAL_SURFACE('',#6046,0.21);
#5202=CYLINDRICAL_SURFACE('',#6065,0.375);
#5203=CYLINDRICAL_SURFACE('',#6076,0.375);
#5204=CYLINDRICAL_SURFACE('',#6082,0.375);
#5205=CYLINDRICAL_SURFACE('',#6088,0.375);
#5206=CYLINDRICAL_SURFACE('',#6096,0.225);
#5207=CYLINDRICAL_SURFACE('',#6098,0.225);
#5208=CYLINDRICAL_SURFACE('',#6100,0.225);
#5209=CYLINDRICAL_SURFACE('',#6102,0.225);
#5210=CYLINDRICAL_SURFACE('',#6104,1.49);
#5211=CYLINDRICAL_SURFACE('',#6109,0.71);
#5212=CYLINDRICAL_SURFACE('',#6110,2.);
#5213=CYLINDRICAL_SURFACE('',#6114,0.375);
#5214=CYLINDRICAL_SURFACE('',#6125,0.375);
#5215=CYLINDRICAL_SURFACE('',#6131,0.375);
#5216=CYLINDRICAL_SURFACE('',#6137,0.375);
#5217=CYLINDRICAL_SURFACE('',#6145,0.225);
#5218=CYLINDRICAL_SURFACE('',#6147,0.225);
#5219=CYLINDRICAL_SURFACE('',#6149,0.225);
#5220=CYLINDRICAL_SURFACE('',#6151,0.225);
#5221=CYLINDRICAL_SURFACE('',#6153,1.49);
#5222=CYLINDRICAL_SURFACE('',#6158,0.71);
#5223=CYLINDRICAL_SURFACE('',#6159,2.);
#5224=CYLINDRICAL_SURFACE('',#6167,0.425);
#5225=CYLINDRICAL_SURFACE('',#6175,0.24505);
#5226=CYLINDRICAL_SURFACE('',#6196,0.976185);
#5227=CYLINDRICAL_SURFACE('',#6198,0.5);
#5228=CYLINDRICAL_SURFACE('',#6204,0.976185);
#5229=CYLINDRICAL_SURFACE('',#6216,1.023815);
#5230=CYLINDRICAL_SURFACE('',#6223,1.5);
#5231=CYLINDRICAL_SURFACE('',#6228,1.023815);
#5232=CYLINDRICAL_SURFACE('',#6250,1.019052);
#5233=CYLINDRICAL_SURFACE('',#6290,0.980948);
#5234=CYLINDRICAL_SURFACE('',#6304,1.013815);
#5235=CYLINDRICAL_SURFACE('',#6308,0.991185);
#5236=CYLINDRICAL_SURFACE('',#6312,1.013815);
#5237=CYLINDRICAL_SURFACE('',#6316,0.991185);
#5238=CYLINDRICAL_SURFACE('',#6324,0.165);
#5239=CYLINDRICAL_SURFACE('',#6328,0.25);
#5240=CYLINDRICAL_SURFACE('',#6331,0.5);
#5241=CYLINDRICAL_SURFACE('',#6347,1.);
#5242=CYLINDRICAL_SURFACE('',#6348,1.);
#5243=CYLINDRICAL_SURFACE('',#6352,0.7);
#5244=CYLINDRICAL_SURFACE('',#6353,0.5);
#5245=CYLINDRICAL_SURFACE('',#6355,0.5);
#5246=CYLINDRICAL_SURFACE('',#6360,0.505);
#5247=CYLINDRICAL_SURFACE('',#6363,0.7);
#5248=CYLINDRICAL_SURFACE('',#6372,0.165);
#5249=CYLINDRICAL_SURFACE('',#6377,0.165);
#5250=CYLINDRICAL_SURFACE('',#6380,0.505);
#5251=CYLINDRICAL_SURFACE('',#6383,0.9);
#5252=CYLINDRICAL_SURFACE('',#6395,0.5);
#5253=CYLINDRICAL_SURFACE('',#6396,0.3);
#5254=CYLINDRICAL_SURFACE('',#6398,0.3);
#5255=CYLINDRICAL_SURFACE('',#6403,0.5);
#5256=CYLINDRICAL_SURFACE('',#6406,0.6);
#5257=CYLINDRICAL_SURFACE('',#6413,1.8);
#5258=CYLINDRICAL_SURFACE('',#6417,0.505);
#5259=CYLINDRICAL_SURFACE('',#6420,0.7);
#5260=CYLINDRICAL_SURFACE('',#6426,0.225);
#5261=CYLINDRICAL_SURFACE('',#6429,0.7);
#5262=CYLINDRICAL_SURFACE('',#6435,0.4);
#5263=CYLINDRICAL_SURFACE('',#6438,1.4);
#5264=CYLINDRICAL_SURFACE('',#6458,0.35);
#5265=CYLINDRICAL_SURFACE('',#6466,0.1954);
#5266=CYLINDRICAL_SURFACE('',#6488,0.165);
#5267=CYLINDRICAL_SURFACE('',#6491,0.165);
#5268=CYLINDRICAL_SURFACE('',#6494,0.165);
#5269=CYLINDRICAL_SURFACE('',#6497,0.165);
#5270=CYLINDRICAL_SURFACE('',#6500,1.82);
#5271=CYLINDRICAL_SURFACE('',#6503,1.82);
#5272=CYLINDRICAL_SURFACE('',#6506,1.82);
#5273=CYLINDRICAL_SURFACE('',#6509,1.82);
#5274=CYLINDRICAL_SURFACE('',#6512,3.);
#5275=CYLINDRICAL_SURFACE('',#6515,3.);
#5276=CYLINDRICAL_SURFACE('',#6518,3.);
#5277=CYLINDRICAL_SURFACE('',#6531,3.);
#5278=CYLINDRICAL_SURFACE('',#6533,3.);
#5279=CYLINDRICAL_SURFACE('',#6552,0.32);
#5280=CYLINDRICAL_SURFACE('',#6553,0.7);
#5281=CYLINDRICAL_SURFACE('',#6562,3.);
#5282=CYLINDRICAL_SURFACE('',#6574,0.32);
#5283=CYLINDRICAL_SURFACE('',#6576,3.);
#5284=CYLINDRICAL_SURFACE('',#6588,0.32);
#5285=CYLINDRICAL_SURFACE('',#6590,3.);
#5286=CYLINDRICAL_SURFACE('',#6597,0.32);
#5287=CYLINDRICAL_SURFACE('',#6602,0.5);
#5288=CYLINDRICAL_SURFACE('',#6606,0.505);
#5289=CYLINDRICAL_SURFACE('',#6609,0.7);
#5290=CYLINDRICAL_SURFACE('',#6618,0.165);
#5291=CYLINDRICAL_SURFACE('',#6623,0.165);
#5292=CYLINDRICAL_SURFACE('',#6626,0.505);
#5293=CYLINDRICAL_SURFACE('',#6629,0.9);
#5294=CYLINDRICAL_SURFACE('',#6648,0.1954);
#5295=ADVANCED_FACE('',(#652),#5172,.F.);
#5296=ADVANCED_FACE('',(#653),#471,.T.);
#5297=ADVANCED_FACE('',(#654),#5173,.F.);
#5298=ADVANCED_FACE('',(#655),#472,.T.);
#5299=ADVANCED_FACE('',(#656),#5174,.F.);
#5300=ADVANCED_FACE('',(#657),#473,.T.);
#5301=ADVANCED_FACE('',(#658),#5175,.F.);
#5302=ADVANCED_FACE('',(#659),#474,.T.);
#5303=ADVANCED_FACE('',(#660),#5176,.F.);
#5304=ADVANCED_FACE('',(#661,#359),#475,.T.);
#5305=ADVANCED_FACE('',(#662,#360),#5177,.F.);
#5306=ADVANCED_FACE('',(#663),#5178,.F.);
#5307=ADVANCED_FACE('',(#664),#476,.T.);
#5308=ADVANCED_FACE('',(#665),#5179,.F.);
#5309=ADVANCED_FACE('',(#666),#477,.T.);
#5310=ADVANCED_FACE('',(#667),#5180,.F.);
#5311=ADVANCED_FACE('',(#668),#478,.T.);
#5312=ADVANCED_FACE('',(#669),#5181,.F.);
#5313=ADVANCED_FACE('',(#670),#479,.T.);
#5314=ADVANCED_FACE('',(#671),#5182,.F.);
#5315=ADVANCED_FACE('',(#672,#361),#480,.T.);
#5316=ADVANCED_FACE('',(#673,#362),#5183,.F.);
#5317=ADVANCED_FACE('',(#674),#5184,.F.);
#5318=ADVANCED_FACE('',(#675,#363),#481,.T.);
#5319=ADVANCED_FACE('',(#676),#5185,.F.);
#5320=ADVANCED_FACE('',(#677,#364),#482,.T.);
#5321=ADVANCED_FACE('',(#678),#5186,.F.);
#5322=ADVANCED_FACE('',(#679,#365),#483,.T.);
#5323=ADVANCED_FACE('',(#680),#5187,.F.);
#5324=ADVANCED_FACE('',(#681,#366),#484,.T.);
#5325=ADVANCED_FACE('',(#682),#5188,.F.);
#5326=ADVANCED_FACE('',(#683),#5189,.F.);
#5327=ADVANCED_FACE('',(#684),#5190,.F.);
#5328=ADVANCED_FACE('',(#685),#5191,.F.);
#5329=ADVANCED_FACE('',(#686,#367),#485,.T.);
#5330=ADVANCED_FACE('',(#687,#368),#486,.T.);
#5331=ADVANCED_FACE('',(#688,#369),#487,.T.);
#5332=ADVANCED_FACE('',(#689,#370),#488,.T.);
#5333=ADVANCED_FACE('',(#690),#489,.T.);
#5334=ADVANCED_FACE('',(#691),#490,.T.);
#5335=ADVANCED_FACE('',(#692),#491,.T.);
#5336=ADVANCED_FACE('',(#693),#492,.T.);
#5337=ADVANCED_FACE('',(#694),#493,.T.);
#5338=ADVANCED_FACE('',(#695),#5192,.F.);
#5339=ADVANCED_FACE('',(#696),#5193,.F.);
#5340=ADVANCED_FACE('',(#697,#371,#372,#373,#374,#375,#376,#377,#378,#379,
#380,#381,#382,#383,#384),#494,.T.);
#5341=ADVANCED_FACE('',(#698,#385,#386),#495,.T.);
#5342=ADVANCED_FACE('',(#699),#5194,.F.);
#5343=ADVANCED_FACE('',(#700),#5195,.F.);
#5344=ADVANCED_FACE('',(#701),#5196,.F.);
#5345=ADVANCED_FACE('',(#702),#5197,.F.);
#5346=ADVANCED_FACE('',(#703),#496,.T.);
#5347=ADVANCED_FACE('',(#704),#497,.T.);
#5348=ADVANCED_FACE('',(#705),#498,.T.);
#5349=ADVANCED_FACE('',(#706),#499,.T.);
#5350=ADVANCED_FACE('',(#707),#5198,.F.);
#5351=ADVANCED_FACE('',(#708),#5199,.F.);
#5352=ADVANCED_FACE('',(#709),#5200,.F.);
#5353=ADVANCED_FACE('',(#710),#5201,.F.);
#5354=ADVANCED_FACE('',(#711,#387,#388,#389,#390,#391),#500,.T.);
#5355=ADVANCED_FACE('',(#712,#392,#393,#394,#395,#396,#397,#398,#399),#501,
 .F.);
#5356=ADVANCED_FACE('',(#713),#502,.T.);
#5357=ADVANCED_FACE('',(#714),#503,.T.);
#5358=ADVANCED_FACE('',(#715),#504,.T.);
#5359=ADVANCED_FACE('',(#716),#505,.T.);
#5360=ADVANCED_FACE('',(#717),#506,.T.);
#5361=ADVANCED_FACE('',(#718),#507,.F.);
#5362=ADVANCED_FACE('',(#719),#508,.T.);
#5363=ADVANCED_FACE('',(#720),#509,.T.);
#5364=ADVANCED_FACE('',(#721),#510,.T.);
#5365=ADVANCED_FACE('',(#722),#511,.T.);
#5366=ADVANCED_FACE('',(#723),#512,.T.);
#5367=ADVANCED_FACE('',(#724),#513,.F.);
#5368=ADVANCED_FACE('',(#725),#5202,.F.);
#5369=ADVANCED_FACE('',(#726,#400),#514,.T.);
#5370=ADVANCED_FACE('',(#727,#401),#515,.T.);
#5371=ADVANCED_FACE('',(#728),#5203,.F.);
#5372=ADVANCED_FACE('',(#729,#402),#516,.T.);
#5373=ADVANCED_FACE('',(#730),#5204,.F.);
#5374=ADVANCED_FACE('',(#731,#403),#517,.T.);
#5375=ADVANCED_FACE('',(#732),#5205,.F.);
#5376=ADVANCED_FACE('',(#733,#404),#518,.T.);
#5377=ADVANCED_FACE('',(#734),#5206,.F.);
#5378=ADVANCED_FACE('',(#735),#5207,.F.);
#5379=ADVANCED_FACE('',(#736),#5208,.F.);
#5380=ADVANCED_FACE('',(#737),#5209,.F.);
#5381=ADVANCED_FACE('',(#738),#5210,.T.);
#5382=ADVANCED_FACE('',(#739,#405),#519,.F.);
#5383=ADVANCED_FACE('',(#740),#5211,.F.);
#5384=ADVANCED_FACE('',(#741),#5212,.T.);
#5385=ADVANCED_FACE('',(#742,#406,#407,#408,#409,#410),#520,.F.);
#5386=ADVANCED_FACE('',(#743),#5213,.F.);
#5387=ADVANCED_FACE('',(#744,#411),#521,.T.);
#5388=ADVANCED_FACE('',(#745,#412),#522,.T.);
#5389=ADVANCED_FACE('',(#746),#5214,.F.);
#5390=ADVANCED_FACE('',(#747,#413),#523,.T.);
#5391=ADVANCED_FACE('',(#748),#5215,.F.);
#5392=ADVANCED_FACE('',(#749,#414),#524,.T.);
#5393=ADVANCED_FACE('',(#750),#5216,.F.);
#5394=ADVANCED_FACE('',(#751,#415),#525,.T.);
#5395=ADVANCED_FACE('',(#752),#5217,.F.);
#5396=ADVANCED_FACE('',(#753),#5218,.F.);
#5397=ADVANCED_FACE('',(#754),#5219,.F.);
#5398=ADVANCED_FACE('',(#755),#5220,.F.);
#5399=ADVANCED_FACE('',(#756),#5221,.T.);
#5400=ADVANCED_FACE('',(#757,#416),#526,.F.);
#5401=ADVANCED_FACE('',(#758),#5222,.F.);
#5402=ADVANCED_FACE('',(#759),#5223,.T.);
#5403=ADVANCED_FACE('',(#760,#417,#418,#419,#420,#421),#527,.F.);
#5404=ADVANCED_FACE('',(#761),#528,.T.);
#5405=ADVANCED_FACE('',(#762),#195,.T.);
#5406=ADVANCED_FACE('',(#763),#5224,.T.);
#5407=ADVANCED_FACE('',(#764),#196,.T.);
#5408=ADVANCED_FACE('',(#765,#422),#529,.T.);
#5409=ADVANCED_FACE('',(#766),#197,.T.);
#5410=ADVANCED_FACE('',(#767),#5225,.T.);
#5411=ADVANCED_FACE('',(#768),#198,.T.);
#5412=ADVANCED_FACE('',(#769),#530,.T.);
#5413=ADVANCED_FACE('',(#770),#531,.F.);
#5414=ADVANCED_FACE('',(#771),#532,.F.);
#5415=ADVANCED_FACE('',(#772),#533,.F.);
#5416=ADVANCED_FACE('',(#773),#534,.F.);
#5417=ADVANCED_FACE('',(#774),#535,.F.);
#5418=ADVANCED_FACE('',(#775),#536,.F.);
#5419=ADVANCED_FACE('',(#776),#537,.F.);
#5420=ADVANCED_FACE('',(#777),#538,.F.);
#5421=ADVANCED_FACE('',(#778),#191,.F.);
#5422=ADVANCED_FACE('',(#779),#5226,.T.);
#5423=ADVANCED_FACE('',(#780),#5227,.F.);
#5424=ADVANCED_FACE('',(#781),#199,.F.);
#5425=ADVANCED_FACE('',(#782,#423),#539,.T.);
#5426=ADVANCED_FACE('',(#783),#5228,.T.);
#5427=ADVANCED_FACE('',(#784,#424),#540,.T.);
#5428=ADVANCED_FACE('',(#785),#200,.F.);
#5429=ADVANCED_FACE('',(#786),#192,.F.);
#5430=ADVANCED_FACE('',(#787),#5229,.F.);
#5431=ADVANCED_FACE('',(#788,#425),#541,.T.);
#5432=ADVANCED_FACE('',(#789),#201,.T.);
#5433=ADVANCED_FACE('',(#790),#5230,.T.);
#5434=ADVANCED_FACE('',(#791),#202,.T.);
#5435=ADVANCED_FACE('',(#792,#426),#542,.T.);
#5436=ADVANCED_FACE('',(#793),#5231,.F.);
#5437=ADVANCED_FACE('',(#794),#175,.T.);
#5438=ADVANCED_FACE('',(#795),#176,.T.);
#5439=ADVANCED_FACE('',(#796),#177,.T.);
#5440=ADVANCED_FACE('',(#797),#178,.T.);
#5441=ADVANCED_FACE('',(#798),#179,.T.);
#5442=ADVANCED_FACE('',(#799),#180,.T.);
#5443=ADVANCED_FACE('',(#800),#181,.T.);
#5444=ADVANCED_FACE('',(#801),#182,.T.);
#5445=ADVANCED_FACE('',(#802),#183,.F.);
#5446=ADVANCED_FACE('',(#803),#5232,.T.);
#5447=ADVANCED_FACE('',(#804),#543,.T.);
#5448=ADVANCED_FACE('',(#805),#184,.F.);
#5449=ADVANCED_FACE('',(#806),#544,.T.);
#5450=ADVANCED_FACE('',(#807),#185,.F.);
#5451=ADVANCED_FACE('',(#808),#545,.T.);
#5452=ADVANCED_FACE('',(#809),#186,.F.);
#5453=ADVANCED_FACE('',(#810),#546,.T.);
#5454=ADVANCED_FACE('',(#811),#187,.F.);
#5455=ADVANCED_FACE('',(#812),#547,.T.);
#5456=ADVANCED_FACE('',(#813),#188,.F.);
#5457=ADVANCED_FACE('',(#814),#548,.T.);
#5458=ADVANCED_FACE('',(#815),#189,.F.);
#5459=ADVANCED_FACE('',(#816),#5233,.F.);
#5460=ADVANCED_FACE('',(#817),#549,.T.);
#5461=ADVANCED_FACE('',(#818),#190,.F.);
#5462=ADVANCED_FACE('',(#819,#427),#550,.T.);
#5463=ADVANCED_FACE('',(#820),#551,.T.);
#5464=ADVANCED_FACE('',(#821,#428),#552,.T.);
#5465=ADVANCED_FACE('',(#822),#5234,.T.);
#5466=ADVANCED_FACE('',(#823,#429),#553,.T.);
#5467=ADVANCED_FACE('',(#824),#5235,.F.);
#5468=ADVANCED_FACE('',(#825,#430),#554,.T.);
#5469=ADVANCED_FACE('',(#826),#5236,.T.);
#5470=ADVANCED_FACE('',(#827,#431),#555,.T.);
#5471=ADVANCED_FACE('',(#828),#5237,.F.);
#5472=ADVANCED_FACE('',(#829),#5238,.F.);
#5473=ADVANCED_FACE('',(#830),#556,.T.);
#5474=ADVANCED_FACE('',(#831),#5239,.F.);
#5475=ADVANCED_FACE('',(#832),#5240,.T.);
#5476=ADVANCED_FACE('',(#833,#432,#433),#557,.F.);
#5477=ADVANCED_FACE('',(#834),#558,.T.);
#5478=ADVANCED_FACE('',(#835),#559,.T.);
#5479=ADVANCED_FACE('',(#836),#560,.T.);
#5480=ADVANCED_FACE('',(#837),#561,.T.);
#5481=ADVANCED_FACE('',(#838),#562,.T.);
#5482=ADVANCED_FACE('',(#839,#434,#435),#563,.T.);
#5483=ADVANCED_FACE('',(#840),#5241,.T.);
#5484=ADVANCED_FACE('',(#841),#5242,.T.);
#5485=ADVANCED_FACE('',(#842,#436),#564,.F.);
#5486=ADVANCED_FACE('',(#843),#5243,.T.);
#5487=ADVANCED_FACE('',(#844),#5244,.T.);
#5488=ADVANCED_FACE('',(#845),#5245,.T.);
#5489=ADVANCED_FACE('',(#846,#437),#565,.T.);
#5490=ADVANCED_FACE('',(#847),#566,.F.);
#5491=ADVANCED_FACE('',(#848),#5246,.F.);
#5492=ADVANCED_FACE('',(#849),#5247,.T.);
#5493=ADVANCED_FACE('',(#850,#438),#567,.T.);
#5494=ADVANCED_FACE('',(#851,#439),#568,.F.);
#5495=ADVANCED_FACE('',(#852),#569,.F.);
#5496=ADVANCED_FACE('',(#853),#5248,.F.);
#5497=ADVANCED_FACE('',(#854),#570,.F.);
#5498=ADVANCED_FACE('',(#855),#571,.F.);
#5499=ADVANCED_FACE('',(#856),#5249,.F.);
#5500=ADVANCED_FACE('',(#857),#572,.F.);
#5501=ADVANCED_FACE('',(#858,#440),#5250,.F.);
#5502=ADVANCED_FACE('',(#859,#441),#5251,.T.);
#5503=ADVANCED_FACE('',(#860,#442),#573,.T.);
#5504=ADVANCED_FACE('',(#861,#443),#574,.F.);
#5505=ADVANCED_FACE('',(#862,#444),#575,.T.);
#5506=ADVANCED_FACE('',(#863,#445),#576,.F.);
#5507=ADVANCED_FACE('',(#864),#5252,.T.);
#5508=ADVANCED_FACE('',(#865),#5253,.T.);
#5509=ADVANCED_FACE('',(#866),#5254,.T.);
#5510=ADVANCED_FACE('',(#867),#577,.T.);
#5511=ADVANCED_FACE('',(#868),#578,.F.);
#5512=ADVANCED_FACE('',(#869),#5255,.F.);
#5513=ADVANCED_FACE('',(#870),#5256,.T.);
#5514=ADVANCED_FACE('',(#871,#446),#579,.F.);
#5515=ADVANCED_FACE('',(#872),#580,.F.);
#5516=ADVANCED_FACE('',(#873),#581,.F.);
#5517=ADVANCED_FACE('',(#874),#5257,.T.);
#5518=ADVANCED_FACE('',(#875,#447),#582,.T.);
#5519=ADVANCED_FACE('',(#876),#5258,.F.);
#5520=ADVANCED_FACE('',(#877),#5259,.T.);
#5521=ADVANCED_FACE('',(#878,#448),#583,.T.);
#5522=ADVANCED_FACE('',(#879,#449),#584,.F.);
#5523=ADVANCED_FACE('',(#880),#5260,.F.);
#5524=ADVANCED_FACE('',(#881),#5261,.T.);
#5525=ADVANCED_FACE('',(#882,#450),#585,.T.);
#5526=ADVANCED_FACE('',(#883,#451),#586,.F.);
#5527=ADVANCED_FACE('',(#884),#5262,.F.);
#5528=ADVANCED_FACE('',(#885),#5263,.T.);
#5529=ADVANCED_FACE('',(#886,#452),#587,.T.);
#5530=ADVANCED_FACE('',(#887,#453),#588,.F.);
#5531=ADVANCED_FACE('',(#888),#589,.F.);
#5532=ADVANCED_FACE('',(#889),#590,.F.);
#5533=ADVANCED_FACE('',(#890),#591,.F.);
#5534=ADVANCED_FACE('',(#891),#592,.F.);
#5535=ADVANCED_FACE('',(#892),#593,.F.);
#5536=ADVANCED_FACE('',(#893),#594,.F.);
#5537=ADVANCED_FACE('',(#894),#595,.F.);
#5538=ADVANCED_FACE('',(#895),#596,.F.);
#5539=ADVANCED_FACE('',(#896),#597,.F.);
#5540=ADVANCED_FACE('',(#897),#598,.T.);
#5541=ADVANCED_FACE('',(#898),#203,.T.);
#5542=ADVANCED_FACE('',(#899),#5264,.T.);
#5543=ADVANCED_FACE('',(#900),#204,.T.);
#5544=ADVANCED_FACE('',(#901,#454),#599,.T.);
#5545=ADVANCED_FACE('',(#902),#205,.T.);
#5546=ADVANCED_FACE('',(#903),#5265,.T.);
#5547=ADVANCED_FACE('',(#904),#5266,.F.);
#5548=ADVANCED_FACE('',(#905),#5267,.F.);
#5549=ADVANCED_FACE('',(#906),#5268,.F.);
#5550=ADVANCED_FACE('',(#907),#5269,.F.);
#5551=ADVANCED_FACE('',(#908),#5270,.F.);
#5552=ADVANCED_FACE('',(#909),#5271,.F.);
#5553=ADVANCED_FACE('',(#910),#5272,.F.);
#5554=ADVANCED_FACE('',(#911),#5273,.F.);
#5555=ADVANCED_FACE('',(#912),#5274,.T.);
#5556=ADVANCED_FACE('',(#913),#5275,.T.);
#5557=ADVANCED_FACE('',(#914),#5276,.T.);
#5558=ADVANCED_FACE('',(#915,#455,#456,#457,#458),#600,.T.);
#5559=ADVANCED_FACE('',(#916),#5277,.T.);
#5560=ADVANCED_FACE('',(#917),#5278,.T.);
#5561=ADVANCED_FACE('',(#918),#601,.F.);
#5562=ADVANCED_FACE('',(#919),#602,.F.);
#5563=ADVANCED_FACE('',(#920),#603,.F.);
#5564=ADVANCED_FACE('',(#921),#604,.F.);
#5565=ADVANCED_FACE('',(#922),#605,.F.);
#5566=ADVANCED_FACE('',(#923,#459),#606,.F.);
#5567=ADVANCED_FACE('',(#924,#460),#607,.F.);
#5568=ADVANCED_FACE('',(#925),#608,.T.);
#5569=ADVANCED_FACE('',(#926),#5279,.F.);
#5570=ADVANCED_FACE('',(#927),#5280,.T.);
#5571=ADVANCED_FACE('',(#928),#609,.F.);
#5572=ADVANCED_FACE('',(#929),#5281,.T.);
#5573=ADVANCED_FACE('',(#930),#610,.F.);
#5574=ADVANCED_FACE('',(#931),#611,.F.);
#5575=ADVANCED_FACE('',(#932),#612,.F.);
#5576=ADVANCED_FACE('',(#933),#613,.F.);
#5577=ADVANCED_FACE('',(#934),#614,.F.);
#5578=ADVANCED_FACE('',(#935,#461),#615,.F.);
#5579=ADVANCED_FACE('',(#936),#616,.T.);
#5580=ADVANCED_FACE('',(#937),#5282,.F.);
#5581=ADVANCED_FACE('',(#938),#617,.F.);
#5582=ADVANCED_FACE('',(#939),#5283,.T.);
#5583=ADVANCED_FACE('',(#940),#618,.F.);
#5584=ADVANCED_FACE('',(#941),#619,.F.);
#5585=ADVANCED_FACE('',(#942),#620,.F.);
#5586=ADVANCED_FACE('',(#943),#621,.F.);
#5587=ADVANCED_FACE('',(#944),#622,.F.);
#5588=ADVANCED_FACE('',(#945,#462),#623,.F.);
#5589=ADVANCED_FACE('',(#946),#624,.T.);
#5590=ADVANCED_FACE('',(#947),#5284,.F.);
#5591=ADVANCED_FACE('',(#948),#625,.F.);
#5592=ADVANCED_FACE('',(#949),#5285,.T.);
#5593=ADVANCED_FACE('',(#950),#626,.F.);
#5594=ADVANCED_FACE('',(#951),#627,.F.);
#5595=ADVANCED_FACE('',(#952),#628,.F.);
#5596=ADVANCED_FACE('',(#953),#629,.F.);
#5597=ADVANCED_FACE('',(#954),#630,.T.);
#5598=ADVANCED_FACE('',(#955),#5286,.F.);
#5599=ADVANCED_FACE('',(#956),#631,.F.);
#5600=ADVANCED_FACE('',(#957),#632,.F.);
#5601=ADVANCED_FACE('',(#958,#463),#633,.F.);
#5602=ADVANCED_FACE('',(#959),#5287,.T.);
#5603=ADVANCED_FACE('',(#960),#634,.F.);
#5604=ADVANCED_FACE('',(#961),#5288,.F.);
#5605=ADVANCED_FACE('',(#962),#5289,.T.);
#5606=ADVANCED_FACE('',(#963,#464),#635,.T.);
#5607=ADVANCED_FACE('',(#964,#465),#636,.F.);
#5608=ADVANCED_FACE('',(#965),#637,.F.);
#5609=ADVANCED_FACE('',(#966),#5290,.F.);
#5610=ADVANCED_FACE('',(#967),#638,.F.);
#5611=ADVANCED_FACE('',(#968),#639,.F.);
#5612=ADVANCED_FACE('',(#969),#5291,.F.);
#5613=ADVANCED_FACE('',(#970),#640,.F.);
#5614=ADVANCED_FACE('',(#971,#466),#5292,.F.);
#5615=ADVANCED_FACE('',(#972,#467),#5293,.T.);
#5616=ADVANCED_FACE('',(#973,#468),#641,.T.);
#5617=ADVANCED_FACE('',(#974,#469),#642,.F.);
#5618=ADVANCED_FACE('',(#975),#643,.F.);
#5619=ADVANCED_FACE('',(#976),#644,.F.);
#5620=ADVANCED_FACE('',(#977),#645,.F.);
#5621=ADVANCED_FACE('',(#978),#646,.F.);
#5622=ADVANCED_FACE('',(#979),#647,.F.);
#5623=ADVANCED_FACE('',(#980),#648,.F.);
#5624=ADVANCED_FACE('',(#981),#649,.F.);
#5625=ADVANCED_FACE('',(#982),#650,.F.);
#5626=ADVANCED_FACE('',(#983,#470),#651,.T.);
#5627=ADVANCED_FACE('',(#984),#206,.T.);
#5628=ADVANCED_FACE('',(#985),#5294,.T.);
#5629=CLOSED_SHELL('',(#5295,#5296,#5297,#5298,#5299,#5300,#5301,#5302,
#5303,#5304,#5305,#5306,#5307,#5308,#5309,#5310,#5311,#5312,#5313,#5314,
#5315,#5316,#5317,#5318,#5319,#5320,#5321,#5322,#5323,#5324,#5325,#5326,
#5327,#5328,#5329,#5330,#5331,#5332,#5333,#5334,#5335,#5336,#5337,#5338,
#5339,#5340,#5341,#5342,#5343,#5344,#5345,#5346,#5347,#5348,#5349,#5350,
#5351,#5352,#5353,#5354,#5355));
#5630=CLOSED_SHELL('',(#5356,#5357,#5358,#5359,#5360,#5361));
#5631=CLOSED_SHELL('',(#5362,#5363,#5364,#5365,#5366,#5367));
#5632=CLOSED_SHELL('',(#5368,#5369,#5370,#5371,#5372,#5373,#5374,#5375,
#5376,#5377,#5378,#5379,#5380,#5381,#5382,#5383,#5384,#5385));
#5633=CLOSED_SHELL('',(#5386,#5387,#5388,#5389,#5390,#5391,#5392,#5393,
#5394,#5395,#5396,#5397,#5398,#5399,#5400,#5401,#5402,#5403));
#5634=CLOSED_SHELL('',(#5404,#5405,#5406,#5407,#5408,#5409,#5410,#5411,
#5412));
#5635=CLOSED_SHELL('',(#5413,#5414,#5415,#5416,#5417,#5418,#5419,#5420));
#5636=CLOSED_SHELL('',(#5421,#5422,#5423,#5424,#5425,#5426,#5427,#5428));
#5637=CLOSED_SHELL('',(#5429,#5430,#5431,#5432,#5433,#5434,#5435,#5436));
#5638=CLOSED_SHELL('',(#5437));
#5639=CLOSED_SHELL('',(#5438));
#5640=CLOSED_SHELL('',(#5439));
#5641=CLOSED_SHELL('',(#5440));
#5642=CLOSED_SHELL('',(#5441));
#5643=CLOSED_SHELL('',(#5442));
#5644=CLOSED_SHELL('',(#5443));
#5645=CLOSED_SHELL('',(#5444));
#5646=CLOSED_SHELL('',(#5445,#5446,#5447,#5448,#5449,#5450,#5451,#5452,
#5453,#5454,#5455,#5456,#5457,#5458,#5459,#5460,#5461,#5462,#5463));
#5647=CLOSED_SHELL('',(#5464,#5465,#5466,#5467));
#5648=CLOSED_SHELL('',(#5468,#5469,#5470,#5471));
#5649=CLOSED_SHELL('',(#5472,#5473,#5474,#5475,#5476,#5477,#5478,#5479,
#5480,#5481,#5482,#5483,#5484,#5485,#5486,#5487,#5488,#5489,#5490));
#5650=CLOSED_SHELL('',(#5491,#5492,#5493,#5494));
#5651=CLOSED_SHELL('',(#5495,#5496,#5497,#5498,#5499,#5500,#5501,#5502,
#5503,#5504));
#5652=CLOSED_SHELL('',(#5505,#5506,#5507,#5508,#5509,#5510,#5511));
#5653=CLOSED_SHELL('',(#5512,#5513,#5514,#5515,#5516,#5517,#5518));
#5654=CLOSED_SHELL('',(#5519,#5520,#5521,#5522));
#5655=CLOSED_SHELL('',(#5523,#5524,#5525,#5526));
#5656=CLOSED_SHELL('',(#5527,#5528,#5529,#5530));
#5657=CLOSED_SHELL('',(#5531,#5532,#5533,#5534,#5535,#5536,#5537,#5538));
#5658=CLOSED_SHELL('',(#5539,#5540,#5541,#5542,#5543,#5544,#5545,#5546));
#5659=CLOSED_SHELL('',(#5547,#5548,#5549,#5550,#5551,#5552,#5553,#5554,
#5555,#5556,#5557,#5558,#5559,#5560,#5561,#5562,#5563,#5564,#5565,#5566,
#5567,#5568,#5569,#5570,#5571,#5572,#5573,#5574,#5575,#5576,#5577,#5578,
#5579,#5580,#5581,#5582,#5583,#5584,#5585,#5586,#5587,#5588,#5589,#5590,
#5591,#5592,#5593,#5594,#5595,#5596,#5597,#5598,#5599,#5600,#5601,#5602,
#5603));
#5660=CLOSED_SHELL('',(#5604,#5605,#5606,#5607));
#5661=CLOSED_SHELL('',(#5608,#5609,#5610,#5611,#5612,#5613,#5614,#5615,
#5616,#5617));
#5662=CLOSED_SHELL('',(#5618,#5619,#5620,#5621,#5622,#5623,#5624,#5625,
#5626,#5627,#5628));
#5663=DERIVED_UNIT_ELEMENT(#5711,1.);
#5664=DERIVED_UNIT_ELEMENT(#10839,-3.);
#5665=DERIVED_UNIT_ELEMENT(#5711,1.);
#5666=DERIVED_UNIT_ELEMENT(#10839,-3.);
#5667=DERIVED_UNIT_ELEMENT(#5711,1.);
#5668=DERIVED_UNIT_ELEMENT(#10839,-3.);
#5669=DERIVED_UNIT_ELEMENT(#5711,1.);
#5670=DERIVED_UNIT_ELEMENT(#10839,-3.);
#5671=DERIVED_UNIT_ELEMENT(#5711,1.);
#5672=DERIVED_UNIT_ELEMENT(#10839,-3.);
#5673=DERIVED_UNIT_ELEMENT(#5711,1.);
#5674=DERIVED_UNIT_ELEMENT(#10839,-3.);
#5675=DERIVED_UNIT_ELEMENT(#5711,1.);
#5676=DERIVED_UNIT_ELEMENT(#10839,-3.);
#5677=DERIVED_UNIT_ELEMENT(#5711,1.);
#5678=DERIVED_UNIT_ELEMENT(#10839,-3.);
#5679=DERIVED_UNIT_ELEMENT(#5711,1.);
#5680=DERIVED_UNIT_ELEMENT(#10839,-3.);
#5681=DERIVED_UNIT_ELEMENT(#5711,1.);
#5682=DERIVED_UNIT_ELEMENT(#10839,-3.);
#5683=DERIVED_UNIT_ELEMENT(#5711,1.);
#5684=DERIVED_UNIT_ELEMENT(#10839,-3.);
#5685=DERIVED_UNIT_ELEMENT(#5711,1.);
#5686=DERIVED_UNIT_ELEMENT(#10839,-3.);
#5687=DERIVED_UNIT_ELEMENT(#5711,1.);
#5688=DERIVED_UNIT_ELEMENT(#10839,-3.);
#5689=DERIVED_UNIT_ELEMENT(#5711,1.);
#5690=DERIVED_UNIT_ELEMENT(#10839,-3.);
#5691=DERIVED_UNIT_ELEMENT(#5711,1.);
#5692=DERIVED_UNIT_ELEMENT(#10839,-3.);
#5693=DERIVED_UNIT_ELEMENT(#5711,1.);
#5694=DERIVED_UNIT_ELEMENT(#10839,-3.);
#5695=DERIVED_UNIT_ELEMENT(#5711,1.);
#5696=DERIVED_UNIT_ELEMENT(#10839,-3.);
#5697=DERIVED_UNIT_ELEMENT(#5711,1.);
#5698=DERIVED_UNIT_ELEMENT(#10839,-3.);
#5699=DERIVED_UNIT_ELEMENT(#5711,1.);
#5700=DERIVED_UNIT_ELEMENT(#10839,-3.);
#5701=DERIVED_UNIT_ELEMENT(#5711,1.);
#5702=DERIVED_UNIT_ELEMENT(#10839,-3.);
#5703=DERIVED_UNIT_ELEMENT(#5711,1.);
#5704=DERIVED_UNIT_ELEMENT(#10839,-3.);
#5705=DERIVED_UNIT_ELEMENT(#5711,1.);
#5706=DERIVED_UNIT_ELEMENT(#10839,-3.);
#5707=DERIVED_UNIT_ELEMENT(#5711,1.);
#5708=DERIVED_UNIT_ELEMENT(#10839,-3.);
#5709=DERIVED_UNIT_ELEMENT(#5711,1.);
#5710=DERIVED_UNIT_ELEMENT(#10839,-3.);
#5711=(
MASS_UNIT()
NAMED_UNIT(*)
SI_UNIT(.KILO.,.GRAM.)
);
#5712=DERIVED_UNIT((#5663,#5664));
#5713=DERIVED_UNIT((#5665,#5666));
#5714=DERIVED_UNIT((#5667,#5668));
#5715=DERIVED_UNIT((#5669,#5670));
#5716=DERIVED_UNIT((#5671,#5672));
#5717=DERIVED_UNIT((#5673,#5674));
#5718=DERIVED_UNIT((#5675,#5676));
#5719=DERIVED_UNIT((#5677,#5678));
#5720=DERIVED_UNIT((#5679,#5680));
#5721=DERIVED_UNIT((#5681,#5682));
#5722=DERIVED_UNIT((#5683,#5684));
#5723=DERIVED_UNIT((#5685,#5686));
#5724=DERIVED_UNIT((#5687,#5688));
#5725=DERIVED_UNIT((#5689,#5690));
#5726=DERIVED_UNIT((#5691,#5692));
#5727=DERIVED_UNIT((#5693,#5694));
#5728=DERIVED_UNIT((#5695,#5696));
#5729=DERIVED_UNIT((#5697,#5698));
#5730=DERIVED_UNIT((#5699,#5700));
#5731=DERIVED_UNIT((#5701,#5702));
#5732=DERIVED_UNIT((#5703,#5704));
#5733=DERIVED_UNIT((#5705,#5706));
#5734=DERIVED_UNIT((#5707,#5708));
#5735=DERIVED_UNIT((#5709,#5710));
#5736=MEASURE_REPRESENTATION_ITEM('density measure',
POSITIVE_RATIO_MEASURE(7850.),#5712);
#5737=MEASURE_REPRESENTATION_ITEM('density measure',
POSITIVE_RATIO_MEASURE(7850.),#5713);
#5738=MEASURE_REPRESENTATION_ITEM('density measure',
POSITIVE_RATIO_MEASURE(7850.),#5714);
#5739=MEASURE_REPRESENTATION_ITEM('density measure',
POSITIVE_RATIO_MEASURE(7850.),#5715);
#5740=MEASURE_REPRESENTATION_ITEM('density measure',
POSITIVE_RATIO_MEASURE(7850.),#5716);
#5741=MEASURE_REPRESENTATION_ITEM('density measure',
POSITIVE_RATIO_MEASURE(7850.),#5717);
#5742=MEASURE_REPRESENTATION_ITEM('density measure',
POSITIVE_RATIO_MEASURE(7850.),#5718);
#5743=MEASURE_REPRESENTATION_ITEM('density measure',
POSITIVE_RATIO_MEASURE(7850.),#5719);
#5744=MEASURE_REPRESENTATION_ITEM('density measure',
POSITIVE_RATIO_MEASURE(7850.),#5720);
#5745=MEASURE_REPRESENTATION_ITEM('density measure',
POSITIVE_RATIO_MEASURE(7850.),#5721);
#5746=MEASURE_REPRESENTATION_ITEM('density measure',
POSITIVE_RATIO_MEASURE(7850.),#5722);
#5747=MEASURE_REPRESENTATION_ITEM('density measure',
POSITIVE_RATIO_MEASURE(7850.),#5723);
#5748=MEASURE_REPRESENTATION_ITEM('density measure',
POSITIVE_RATIO_MEASURE(7850.),#5724);
#5749=MEASURE_REPRESENTATION_ITEM('density measure',
POSITIVE_RATIO_MEASURE(7850.),#5725);
#5750=MEASURE_REPRESENTATION_ITEM('density measure',
POSITIVE_RATIO_MEASURE(7850.),#5726);
#5751=MEASURE_REPRESENTATION_ITEM('density measure',
POSITIVE_RATIO_MEASURE(7850.),#5727);
#5752=MEASURE_REPRESENTATION_ITEM('density measure',
POSITIVE_RATIO_MEASURE(7850.),#5728);
#5753=MEASURE_REPRESENTATION_ITEM('density measure',
POSITIVE_RATIO_MEASURE(7850.),#5729);
#5754=MEASURE_REPRESENTATION_ITEM('density measure',
POSITIVE_RATIO_MEASURE(7850.),#5730);
#5755=MEASURE_REPRESENTATION_ITEM('density measure',
POSITIVE_RATIO_MEASURE(7850.),#5731);
#5756=MEASURE_REPRESENTATION_ITEM('density measure',
POSITIVE_RATIO_MEASURE(7850.),#5732);
#5757=MEASURE_REPRESENTATION_ITEM('density measure',
POSITIVE_RATIO_MEASURE(7850.),#5733);
#5758=MEASURE_REPRESENTATION_ITEM('density measure',
POSITIVE_RATIO_MEASURE(7850.),#5734);
#5759=MEASURE_REPRESENTATION_ITEM('density measure',
POSITIVE_RATIO_MEASURE(7850.),#5735);
#5760=PROPERTY_DEFINITION_REPRESENTATION(#5880,#5808);
#5761=PROPERTY_DEFINITION_REPRESENTATION(#5881,#5809);
#5762=PROPERTY_DEFINITION_REPRESENTATION(#5882,#5810);
#5763=PROPERTY_DEFINITION_REPRESENTATION(#5883,#5811);
#5764=PROPERTY_DEFINITION_REPRESENTATION(#5884,#5812);
#5765=PROPERTY_DEFINITION_REPRESENTATION(#5885,#5813);
#5766=PROPERTY_DEFINITION_REPRESENTATION(#5886,#5814);
#5767=PROPERTY_DEFINITION_REPRESENTATION(#5887,#5815);
#5768=PROPERTY_DEFINITION_REPRESENTATION(#5888,#5816);
#5769=PROPERTY_DEFINITION_REPRESENTATION(#5889,#5817);
#5770=PROPERTY_DEFINITION_REPRESENTATION(#5890,#5818);
#5771=PROPERTY_DEFINITION_REPRESENTATION(#5891,#5819);
#5772=PROPERTY_DEFINITION_REPRESENTATION(#5892,#5820);
#5773=PROPERTY_DEFINITION_REPRESENTATION(#5893,#5821);
#5774=PROPERTY_DEFINITION_REPRESENTATION(#5894,#5822);
#5775=PROPERTY_DEFINITION_REPRESENTATION(#5895,#5823);
#5776=PROPERTY_DEFINITION_REPRESENTATION(#5896,#5824);
#5777=PROPERTY_DEFINITION_REPRESENTATION(#5897,#5825);
#5778=PROPERTY_DEFINITION_REPRESENTATION(#5898,#5826);
#5779=PROPERTY_DEFINITION_REPRESENTATION(#5899,#5827);
#5780=PROPERTY_DEFINITION_REPRESENTATION(#5900,#5828);
#5781=PROPERTY_DEFINITION_REPRESENTATION(#5901,#5829);
#5782=PROPERTY_DEFINITION_REPRESENTATION(#5902,#5830);
#5783=PROPERTY_DEFINITION_REPRESENTATION(#5903,#5831);
#5784=PROPERTY_DEFINITION_REPRESENTATION(#5904,#5832);
#5785=PROPERTY_DEFINITION_REPRESENTATION(#5905,#5833);
#5786=PROPERTY_DEFINITION_REPRESENTATION(#5906,#5834);
#5787=PROPERTY_DEFINITION_REPRESENTATION(#5907,#5835);
#5788=PROPERTY_DEFINITION_REPRESENTATION(#5908,#5836);
#5789=PROPERTY_DEFINITION_REPRESENTATION(#5909,#5837);
#5790=PROPERTY_DEFINITION_REPRESENTATION(#5910,#5838);
#5791=PROPERTY_DEFINITION_REPRESENTATION(#5911,#5839);
#5792=PROPERTY_DEFINITION_REPRESENTATION(#5912,#5840);
#5793=PROPERTY_DEFINITION_REPRESENTATION(#5913,#5841);
#5794=PROPERTY_DEFINITION_REPRESENTATION(#5914,#5842);
#5795=PROPERTY_DEFINITION_REPRESENTATION(#5915,#5843);
#5796=PROPERTY_DEFINITION_REPRESENTATION(#5916,#5844);
#5797=PROPERTY_DEFINITION_REPRESENTATION(#5917,#5845);
#5798=PROPERTY_DEFINITION_REPRESENTATION(#5918,#5846);
#5799=PROPERTY_DEFINITION_REPRESENTATION(#5919,#5847);
#5800=PROPERTY_DEFINITION_REPRESENTATION(#5920,#5848);
#5801=PROPERTY_DEFINITION_REPRESENTATION(#5921,#5849);
#5802=PROPERTY_DEFINITION_REPRESENTATION(#5922,#5850);
#5803=PROPERTY_DEFINITION_REPRESENTATION(#5923,#5851);
#5804=PROPERTY_DEFINITION_REPRESENTATION(#5924,#5852);
#5805=PROPERTY_DEFINITION_REPRESENTATION(#5925,#5853);
#5806=PROPERTY_DEFINITION_REPRESENTATION(#5926,#5854);
#5807=PROPERTY_DEFINITION_REPRESENTATION(#5927,#5855);
#5808=REPRESENTATION('material name',(#5856),#10810);
#5809=REPRESENTATION('density',(#5736),#10810);
#5810=REPRESENTATION('material name',(#5857),#10811);
#5811=REPRESENTATION('density',(#5737),#10811);
#5812=REPRESENTATION('material name',(#5858),#10812);
#5813=REPRESENTATION('density',(#5738),#10812);
#5814=REPRESENTATION('material name',(#5859),#10813);
#5815=REPRESENTATION('density',(#5739),#10813);
#5816=REPRESENTATION('material name',(#5860),#10814);
#5817=REPRESENTATION('density',(#5740),#10814);
#5818=REPRESENTATION('material name',(#5861),#10815);
#5819=REPRESENTATION('density',(#5741),#10815);
#5820=REPRESENTATION('material name',(#5862),#10817);
#5821=REPRESENTATION('density',(#5742),#10817);
#5822=REPRESENTATION('material name',(#5863),#10818);
#5823=REPRESENTATION('density',(#5743),#10818);
#5824=REPRESENTATION('material name',(#5864),#10819);
#5825=REPRESENTATION('density',(#5744),#10819);
#5826=REPRESENTATION('material name',(#5865),#10820);
#5827=REPRESENTATION('density',(#5745),#10820);
#5828=REPRESENTATION('material name',(#5866),#10821);
#5829=REPRESENTATION('density',(#5746),#10821);
#5830=REPRESENTATION('material name',(#5867),#10823);
#5831=REPRESENTATION('density',(#5747),#10823);
#5832=REPRESENTATION('material name',(#5868),#10824);
#5833=REPRESENTATION('density',(#5748),#10824);
#5834=REPRESENTATION('material name',(#5869),#10825);
#5835=REPRESENTATION('density',(#5749),#10825);
#5836=REPRESENTATION('material name',(#5870),#10826);
#5837=REPRESENTATION('density',(#5750),#10826);
#5838=REPRESENTATION('material name',(#5871),#10827);
#5839=REPRESENTATION('density',(#5751),#10827);
#5840=REPRESENTATION('material name',(#5872),#10828);
#5841=REPRESENTATION('density',(#5752),#10828);
#5842=REPRESENTATION('material name',(#5873),#10829);
#5843=REPRESENTATION('density',(#5753),#10829);
#5844=REPRESENTATION('material name',(#5874),#10830);
#5845=REPRESENTATION('density',(#5754),#10830);
#5846=REPRESENTATION('material name',(#5875),#10831);
#5847=REPRESENTATION('density',(#5755),#10831);
#5848=REPRESENTATION('material name',(#5876),#10833);
#5849=REPRESENTATION('density',(#5756),#10833);
#5850=REPRESENTATION('material name',(#5877),#10834);
#5851=REPRESENTATION('density',(#5757),#10834);
#5852=REPRESENTATION('material name',(#5878),#10835);
#5853=REPRESENTATION('density',(#5758),#10835);
#5854=REPRESENTATION('material name',(#5879),#10836);
#5855=REPRESENTATION('density',(#5759),#10836);
#5856=DESCRIPTIVE_REPRESENTATION_ITEM('Steel','Steel');
#5857=DESCRIPTIVE_REPRESENTATION_ITEM('Steel','Steel');
#5858=DESCRIPTIVE_REPRESENTATION_ITEM('Steel','Steel');
#5859=DESCRIPTIVE_REPRESENTATION_ITEM('Steel','Steel');
#5860=DESCRIPTIVE_REPRESENTATION_ITEM('Steel','Steel');
#5861=DESCRIPTIVE_REPRESENTATION_ITEM('Steel','Steel');
#5862=DESCRIPTIVE_REPRESENTATION_ITEM('Steel','Steel');
#5863=DESCRIPTIVE_REPRESENTATION_ITEM('Steel','Steel');
#5864=DESCRIPTIVE_REPRESENTATION_ITEM('Steel','Steel');
#5865=DESCRIPTIVE_REPRESENTATION_ITEM('Steel','Steel');
#5866=DESCRIPTIVE_REPRESENTATION_ITEM('Steel','Steel');
#5867=DESCRIPTIVE_REPRESENTATION_ITEM('Steel','Steel');
#5868=DESCRIPTIVE_REPRESENTATION_ITEM('Steel','Steel');
#5869=DESCRIPTIVE_REPRESENTATION_ITEM('Steel','Steel');
#5870=DESCRIPTIVE_REPRESENTATION_ITEM('Steel','Steel');
#5871=DESCRIPTIVE_REPRESENTATION_ITEM('Steel','Steel');
#5872=DESCRIPTIVE_REPRESENTATION_ITEM('Steel','Steel');
#5873=DESCRIPTIVE_REPRESENTATION_ITEM('Steel','Steel');
#5874=DESCRIPTIVE_REPRESENTATION_ITEM('Steel','Steel');
#5875=DESCRIPTIVE_REPRESENTATION_ITEM('Steel','Steel');
#5876=DESCRIPTIVE_REPRESENTATION_ITEM('Steel','Steel');
#5877=DESCRIPTIVE_REPRESENTATION_ITEM('Steel','Steel');
#5878=DESCRIPTIVE_REPRESENTATION_ITEM('Steel','Steel');
#5879=DESCRIPTIVE_REPRESENTATION_ITEM('Steel','Steel');
#5880=PROPERTY_DEFINITION('material property','material name',#10973);
#5881=PROPERTY_DEFINITION('material property','density of part',#10973);
#5882=PROPERTY_DEFINITION('material property','material name',#10974);
#5883=PROPERTY_DEFINITION('material property','density of part',#10974);
#5884=PROPERTY_DEFINITION('material property','material name',#10975);
#5885=PROPERTY_DEFINITION('material property','density of part',#10975);
#5886=PROPERTY_DEFINITION('material property','material name',#10976);
#5887=PROPERTY_DEFINITION('material property','density of part',#10976);
#5888=PROPERTY_DEFINITION('material property','material name',#10977);
#5889=PROPERTY_DEFINITION('material property','density of part',#10977);
#5890=PROPERTY_DEFINITION('material property','material name',#10978);
#5891=PROPERTY_DEFINITION('material property','density of part',#10978);
#5892=PROPERTY_DEFINITION('material property','material name',#10980);
#5893=PROPERTY_DEFINITION('material property','density of part',#10980);
#5894=PROPERTY_DEFINITION('material property','material name',#10981);
#5895=PROPERTY_DEFINITION('material property','density of part',#10981);
#5896=PROPERTY_DEFINITION('material property','material name',#10982);
#5897=PROPERTY_DEFINITION('material property','density of part',#10982);
#5898=PROPERTY_DEFINITION('material property','material name',#10983);
#5899=PROPERTY_DEFINITION('material property','density of part',#10983);
#5900=PROPERTY_DEFINITION('material property','material name',#10984);
#5901=PROPERTY_DEFINITION('material property','density of part',#10984);
#5902=PROPERTY_DEFINITION('material property','material name',#10986);
#5903=PROPERTY_DEFINITION('material property','density of part',#10986);
#5904=PROPERTY_DEFINITION('material property','material name',#10987);
#5905=PROPERTY_DEFINITION('material property','density of part',#10987);
#5906=PROPERTY_DEFINITION('material property','material name',#10988);
#5907=PROPERTY_DEFINITION('material property','density of part',#10988);
#5908=PROPERTY_DEFINITION('material property','material name',#10989);
#5909=PROPERTY_DEFINITION('material property','density of part',#10989);
#5910=PROPERTY_DEFINITION('material property','material name',#10990);
#5911=PROPERTY_DEFINITION('material property','density of part',#10990);
#5912=PROPERTY_DEFINITION('material property','material name',#10991);
#5913=PROPERTY_DEFINITION('material property','density of part',#10991);
#5914=PROPERTY_DEFINITION('material property','material name',#10992);
#5915=PROPERTY_DEFINITION('material property','density of part',#10992);
#5916=PROPERTY_DEFINITION('material property','material name',#10993);
#5917=PROPERTY_DEFINITION('material property','density of part',#10993);
#5918=PROPERTY_DEFINITION('material property','material name',#10994);
#5919=PROPERTY_DEFINITION('material property','density of part',#10994);
#5920=PROPERTY_DEFINITION('material property','material name',#10996);
#5921=PROPERTY_DEFINITION('material property','density of part',#10996);
#5922=PROPERTY_DEFINITION('material property','material name',#10997);
#5923=PROPERTY_DEFINITION('material property','density of part',#10997);
#5924=PROPERTY_DEFINITION('material property','material name',#10998);
#5925=PROPERTY_DEFINITION('material property','density of part',#10998);
#5926=PROPERTY_DEFINITION('material property','material name',#10999);
#5927=PROPERTY_DEFINITION('material property','density of part',#10999);
#5928=AXIS2_PLACEMENT_3D('',#8500,#6666,#6667);
#5929=AXIS2_PLACEMENT_3D('',#8501,#6668,#6669);
#5930=AXIS2_PLACEMENT_3D('',#8502,#6670,#6671);
#5931=AXIS2_PLACEMENT_3D('',#8503,#6672,#6673);
#5932=AXIS2_PLACEMENT_3D('',#8505,#6674,#6675);
#5933=AXIS2_PLACEMENT_3D('',#8508,#6677,#6678);
#5934=AXIS2_PLACEMENT_3D('',#8509,#6679,#6680);
#5935=AXIS2_PLACEMENT_3D('',#8510,#6681,#6682);
#5936=AXIS2_PLACEMENT_3D('',#8512,#6683,#6684);
#5937=AXIS2_PLACEMENT_3D('',#8515,#6686,#6687);
#5938=AXIS2_PLACEMENT_3D('',#8516,#6688,#6689);
#5939=AXIS2_PLACEMENT_3D('',#8517,#6690,#6691);
#5940=AXIS2_PLACEMENT_3D('',#8519,#6692,#6693);
#5941=AXIS2_PLACEMENT_3D('',#8522,#6695,#6696);
#5942=AXIS2_PLACEMENT_3D('',#8523,#6697,#6698);
#5943=AXIS2_PLACEMENT_3D('',#8524,#6699,#6700);
#5944=AXIS2_PLACEMENT_3D('',#8526,#6701,#6702);
#5945=AXIS2_PLACEMENT_3D('',#8529,#6704,#6705);
#5946=AXIS2_PLACEMENT_3D('',#8530,#6706,#6707);
#5947=AXIS2_PLACEMENT_3D('',#8531,#6708,#6709);
#5948=AXIS2_PLACEMENT_3D('',#8533,#6710,#6711);
#5949=AXIS2_PLACEMENT_3D('',#8536,#6713,#6714);
#5950=AXIS2_PLACEMENT_3D('',#8537,#6715,#6716);
#5951=AXIS2_PLACEMENT_3D('',#8539,#6717,#6718);
#5952=AXIS2_PLACEMENT_3D('',#8540,#6719,#6720);
#5953=AXIS2_PLACEMENT_3D('',#8542,#6721,#6722);
#5954=AXIS2_PLACEMENT_3D('',#8579,#6724,#6725);
#5955=AXIS2_PLACEMENT_3D('',#8581,#6726,#6727);
#5956=AXIS2_PLACEMENT_3D('',#8584,#6729,#6730);
#5957=AXIS2_PLACEMENT_3D('',#8585,#6731,#6732);
#5958=AXIS2_PLACEMENT_3D('',#8586,#6733,#6734);
#5959=AXIS2_PLACEMENT_3D('',#8588,#6735,#6736);
#5960=AXIS2_PLACEMENT_3D('',#8591,#6738,#6739);
#5961=AXIS2_PLACEMENT_3D('',#8592,#6740,#6741);
#5962=AXIS2_PLACEMENT_3D('',#8593,#6742,#6743);
#5963=AXIS2_PLACEMENT_3D('',#8595,#6744,#6745);
#5964=AXIS2_PLACEMENT_3D('',#8598,#6747,#6748);
#5965=AXIS2_PLACEMENT_3D('',#8599,#6749,#6750);
#5966=AXIS2_PLACEMENT_3D('',#8600,#6751,#6752);
#5967=AXIS2_PLACEMENT_3D('',#8602,#6753,#6754);
#5968=AXIS2_PLACEMENT_3D('',#8605,#6756,#6757);
#5969=AXIS2_PLACEMENT_3D('',#8606,#6758,#6759);
#5970=AXIS2_PLACEMENT_3D('',#8607,#6760,#6761);
#5971=AXIS2_PLACEMENT_3D('',#8609,#6762,#6763);
#5972=AXIS2_PLACEMENT_3D('',#8612,#6765,#6766);
#5973=AXIS2_PLACEMENT_3D('',#8613,#6767,#6768);
#5974=AXIS2_PLACEMENT_3D('',#8615,#6769,#6770);
#5975=AXIS2_PLACEMENT_3D('',#8616,#6771,#6772);
#5976=AXIS2_PLACEMENT_3D('',#8618,#6773,#6774);
#5977=AXIS2_PLACEMENT_3D('',#8655,#6776,#6777);
#5978=AXIS2_PLACEMENT_3D('',#8657,#6778,#6779);
#5979=AXIS2_PLACEMENT_3D('',#8660,#6781,#6782);
#5980=AXIS2_PLACEMENT_3D('',#8661,#6783,#6784);
#5981=AXIS2_PLACEMENT_3D('',#8663,#6785,#6786);
#5982=AXIS2_PLACEMENT_3D('',#8664,#6787,#6788);
#5983=AXIS2_PLACEMENT_3D('',#8666,#6789,#6790);
#5984=AXIS2_PLACEMENT_3D('',#8669,#6792,#6793);
#5985=AXIS2_PLACEMENT_3D('',#8670,#6794,#6795);
#5986=AXIS2_PLACEMENT_3D('',#8672,#6796,#6797);
#5987=AXIS2_PLACEMENT_3D('',#8673,#6798,#6799);
#5988=AXIS2_PLACEMENT_3D('',#8675,#6800,#6801);
#5989=AXIS2_PLACEMENT_3D('',#8678,#6803,#6804);
#5990=AXIS2_PLACEMENT_3D('',#8679,#6805,#6806);
#5991=AXIS2_PLACEMENT_3D('',#8681,#6807,#6808);
#5992=AXIS2_PLACEMENT_3D('',#8682,#6809,#6810);
#5993=AXIS2_PLACEMENT_3D('',#8684,#6811,#6812);
#5994=AXIS2_PLACEMENT_3D('',#8687,#6814,#6815);
#5995=AXIS2_PLACEMENT_3D('',#8688,#6816,#6817);
#5996=AXIS2_PLACEMENT_3D('',#8690,#6818,#6819);
#5997=AXIS2_PLACEMENT_3D('',#8691,#6820,#6821);
#5998=AXIS2_PLACEMENT_3D('',#8693,#6822,#6823);
#5999=AXIS2_PLACEMENT_3D('',#8695,#6825,#6826);
#6000=AXIS2_PLACEMENT_3D('',#8697,#6827,#6828);
#6001=AXIS2_PLACEMENT_3D('',#8699,#6830,#6831);
#6002=AXIS2_PLACEMENT_3D('',#8701,#6832,#6833);
#6003=AXIS2_PLACEMENT_3D('',#8703,#6835,#6836);
#6004=AXIS2_PLACEMENT_3D('',#8705,#6837,#6838);
#6005=AXIS2_PLACEMENT_3D('',#8707,#6840,#6841);
#6006=AXIS2_PLACEMENT_3D('',#8709,#6842,#6843);
#6007=AXIS2_PLACEMENT_3D('',#8710,#6844,#6845);
#6008=AXIS2_PLACEMENT_3D('',#8712,#6846,#6847);
#6009=AXIS2_PLACEMENT_3D('',#8713,#6848,#6849);
#6010=AXIS2_PLACEMENT_3D('',#8715,#6850,#6851);
#6011=AXIS2_PLACEMENT_3D('',#8716,#6852,#6853);
#6012=AXIS2_PLACEMENT_3D('',#8718,#6854,#6855);
#6013=AXIS2_PLACEMENT_3D('',#8719,#6856,#6857);
#6014=AXIS2_PLACEMENT_3D('',#8720,#6858,#6859);
#6015=AXIS2_PLACEMENT_3D('',#8721,#6860,#6861);
#6016=AXIS2_PLACEMENT_3D('',#8730,#6866,#6867);
#6017=AXIS2_PLACEMENT_3D('',#8736,#6871,#6872);
#6018=AXIS2_PLACEMENT_3D('',#8742,#6876,#6877);
#6019=AXIS2_PLACEMENT_3D('',#8744,#6878,#6879);
#6020=AXIS2_PLACEMENT_3D('',#8746,#6881,#6882);
#6021=AXIS2_PLACEMENT_3D('',#8748,#6883,#6884);
#6022=AXIS2_PLACEMENT_3D('',#8750,#6886,#6887);
#6023=AXIS2_PLACEMENT_3D('',#8752,#6889,#6890);
#6024=AXIS2_PLACEMENT_3D('',#8754,#6892,#6893);
#6025=AXIS2_PLACEMENT_3D('',#8756,#6894,#6895);
#6026=AXIS2_PLACEMENT_3D('',#8759,#6897,#6898);
#6027=AXIS2_PLACEMENT_3D('',#8760,#6899,#6900);
#6028=AXIS2_PLACEMENT_3D('',#8762,#6901,#6902);
#6029=AXIS2_PLACEMENT_3D('',#8765,#6904,#6905);
#6030=AXIS2_PLACEMENT_3D('',#8766,#6906,#6907);
#6031=AXIS2_PLACEMENT_3D('',#8768,#6908,#6909);
#6032=AXIS2_PLACEMENT_3D('',#8771,#6911,#6912);
#6033=AXIS2_PLACEMENT_3D('',#8772,#6913,#6914);
#6034=AXIS2_PLACEMENT_3D('',#8774,#6915,#6916);
#6035=AXIS2_PLACEMENT_3D('',#8777,#6918,#6919);
#6036=AXIS2_PLACEMENT_3D('',#8778,#6920,#6921);
#6037=AXIS2_PLACEMENT_3D('',#8787,#6926,#6927);
#6038=AXIS2_PLACEMENT_3D('',#8793,#6931,#6932);
#6039=AXIS2_PLACEMENT_3D('',#8799,#6936,#6937);
#6040=AXIS2_PLACEMENT_3D('',#8802,#6940,#6941);
#6041=AXIS2_PLACEMENT_3D('',#8804,#6942,#6943);
#6042=AXIS2_PLACEMENT_3D('',#8806,#6945,#6946);
#6043=AXIS2_PLACEMENT_3D('',#8808,#6947,#6948);
#6044=AXIS2_PLACEMENT_3D('',#8810,#6950,#6951);
#6045=AXIS2_PLACEMENT_3D('',#8812,#6952,#6953);
#6046=AXIS2_PLACEMENT_3D('',#8814,#6955,#6956);
#6047=AXIS2_PLACEMENT_3D('',#8816,#6957,#6958);
#6048=AXIS2_PLACEMENT_3D('',#8818,#6960,#6961);
#6049=AXIS2_PLACEMENT_3D('',#8819,#6962,#6963);
#6050=AXIS2_PLACEMENT_3D('',#8820,#6964,#6965);
#6051=AXIS2_PLACEMENT_3D('',#8821,#6966,#6967);
#6052=AXIS2_PLACEMENT_3D('',#8830,#6972,#6973);
#6053=AXIS2_PLACEMENT_3D('',#8836,#6977,#6978);
#6054=AXIS2_PLACEMENT_3D('',#8842,#6982,#6983);
#6055=AXIS2_PLACEMENT_3D('',#8845,#6986,#6987);
#6056=AXIS2_PLACEMENT_3D('',#8846,#6988,#6989);
#6057=AXIS2_PLACEMENT_3D('',#8847,#6990,#6991);
#6058=AXIS2_PLACEMENT_3D('',#8848,#6992,#6993);
#6059=AXIS2_PLACEMENT_3D('',#8857,#6998,#6999);
#6060=AXIS2_PLACEMENT_3D('',#8863,#7003,#7004);
#6061=AXIS2_PLACEMENT_3D('',#8869,#7008,#7009);
#6062=AXIS2_PLACEMENT_3D('',#8872,#7012,#7013);
#6063=AXIS2_PLACEMENT_3D('',#8873,#7014,#7015);
#6064=AXIS2_PLACEMENT_3D('',#8874,#7016,#7017);
#6065=AXIS2_PLACEMENT_3D('',#8875,#7018,#7019);
#6066=AXIS2_PLACEMENT_3D('',#8880,#7021,#7022);
#6067=AXIS2_PLACEMENT_3D('',#8883,#7024,#7025);
#6068=AXIS2_PLACEMENT_3D('',#8884,#7026,#7027);
#6069=AXIS2_PLACEMENT_3D('',#8886,#7028,#7029);
#6070=AXIS2_PLACEMENT_3D('',#8887,#7030,#7031);
#6071=AXIS2_PLACEMENT_3D('',#8889,#7032,#7033);
#6072=AXIS2_PLACEMENT_3D('',#8890,#7034,#7035);
#6073=AXIS2_PLACEMENT_3D('',#8893,#7036,#7037);
#6074=AXIS2_PLACEMENT_3D('',#8894,#7038,#7039);
#6075=AXIS2_PLACEMENT_3D('',#8896,#7040,#7041);
#6076=AXIS2_PLACEMENT_3D('',#8897,#7042,#7043);
#6077=AXIS2_PLACEMENT_3D('',#8901,#7045,#7046);
#6078=AXIS2_PLACEMENT_3D('',#8903,#7048,#7049);
#6079=AXIS2_PLACEMENT_3D('',#8906,#7050,#7051);
#6080=AXIS2_PLACEMENT_3D('',#8907,#7052,#7053);
#6081=AXIS2_PLACEMENT_3D('',#8909,#7054,#7055);
#6082=AXIS2_PLACEMENT_3D('',#8910,#7056,#7057);
#6083=AXIS2_PLACEMENT_3D('',#8914,#7059,#7060);
#6084=AXIS2_PLACEMENT_3D('',#8916,#7062,#7063);
#6085=AXIS2_PLACEMENT_3D('',#8919,#7064,#7065);
#6086=AXIS2_PLACEMENT_3D('',#8920,#7066,#7067);
#6087=AXIS2_PLACEMENT_3D('',#8922,#7068,#7069);
#6088=AXIS2_PLACEMENT_3D('',#8923,#7070,#7071);
#6089=AXIS2_PLACEMENT_3D('',#8927,#7073,#7074);
#6090=AXIS2_PLACEMENT_3D('',#8929,#7076,#7077);
#6091=AXIS2_PLACEMENT_3D('',#8930,#7078,#7079);
#6092=AXIS2_PLACEMENT_3D('',#8931,#7080,#7081);
#6093=AXIS2_PLACEMENT_3D('',#8932,#7082,#7083);
#6094=AXIS2_PLACEMENT_3D('',#8933,#7084,#7085);
#6095=AXIS2_PLACEMENT_3D('',#8935,#7086,#7087);
#6096=AXIS2_PLACEMENT_3D('',#8936,#7088,#7089);
#6097=AXIS2_PLACEMENT_3D('',#8938,#7090,#7091);
#6098=AXIS2_PLACEMENT_3D('',#8940,#7093,#7094);
#6099=AXIS2_PLACEMENT_3D('',#8942,#7095,#7096);
#6100=AXIS2_PLACEMENT_3D('',#8944,#7098,#7099);
#6101=AXIS2_PLACEMENT_3D('',#8946,#7100,#7101);
#6102=AXIS2_PLACEMENT_3D('',#8948,#7103,#7104);
#6103=AXIS2_PLACEMENT_3D('',#8950,#7105,#7106);
#6104=AXIS2_PLACEMENT_3D('',#8952,#7108,#7109);
#6105=AXIS2_PLACEMENT_3D('',#8954,#7110,#7111);
#6106=AXIS2_PLACEMENT_3D('',#8957,#7113,#7114);
#6107=AXIS2_PLACEMENT_3D('',#8958,#7115,#7116);
#6108=AXIS2_PLACEMENT_3D('',#8960,#7117,#7118);
#6109=AXIS2_PLACEMENT_3D('',#8961,#7119,#7120);
#6110=AXIS2_PLACEMENT_3D('',#8963,#7122,#7123);
#6111=AXIS2_PLACEMENT_3D('',#8966,#7125,#7126);
#6112=AXIS2_PLACEMENT_3D('',#8967,#7127,#7128);
#6113=AXIS2_PLACEMENT_3D('',#8968,#7129,#7130);
#6114=AXIS2_PLACEMENT_3D('',#8969,#7131,#7132);
#6115=AXIS2_PLACEMENT_3D('',#8974,#7134,#7135);
#6116=AXIS2_PLACEMENT_3D('',#8977,#7137,#7138);
#6117=AXIS2_PLACEMENT_3D('',#8978,#7139,#7140);
#6118=AXIS2_PLACEMENT_3D('',#8980,#7141,#7142);
#6119=AXIS2_PLACEMENT_3D('',#8981,#7143,#7144);
#6120=AXIS2_PLACEMENT_3D('',#8983,#7145,#7146);
#6121=AXIS2_PLACEMENT_3D('',#8984,#7147,#7148);
#6122=AXIS2_PLACEMENT_3D('',#8987,#7149,#7150);
#6123=AXIS2_PLACEMENT_3D('',#8988,#7151,#7152);
#6124=AXIS2_PLACEMENT_3D('',#8990,#7153,#7154);
#6125=AXIS2_PLACEMENT_3D('',#8991,#7155,#7156);
#6126=AXIS2_PLACEMENT_3D('',#8995,#7158,#7159);
#6127=AXIS2_PLACEMENT_3D('',#8997,#7161,#7162);
#6128=AXIS2_PLACEMENT_3D('',#9000,#7163,#7164);
#6129=AXIS2_PLACEMENT_3D('',#9001,#7165,#7166);
#6130=AXIS2_PLACEMENT_3D('',#9003,#7167,#7168);
#6131=AXIS2_PLACEMENT_3D('',#9004,#7169,#7170);
#6132=AXIS2_PLACEMENT_3D('',#9008,#7172,#7173);
#6133=AXIS2_PLACEMENT_3D('',#9010,#7175,#7176);
#6134=AXIS2_PLACEMENT_3D('',#9013,#7177,#7178);
#6135=AXIS2_PLACEMENT_3D('',#9014,#7179,#7180);
#6136=AXIS2_PLACEMENT_3D('',#9016,#7181,#7182);
#6137=AXIS2_PLACEMENT_3D('',#9017,#7183,#7184);
#6138=AXIS2_PLACEMENT_3D('',#9021,#7186,#7187);
#6139=AXIS2_PLACEMENT_3D('',#9023,#7189,#7190);
#6140=AXIS2_PLACEMENT_3D('',#9024,#7191,#7192);
#6141=AXIS2_PLACEMENT_3D('',#9025,#7193,#7194);
#6142=AXIS2_PLACEMENT_3D('',#9026,#7195,#7196);
#6143=AXIS2_PLACEMENT_3D('',#9027,#7197,#7198);
#6144=AXIS2_PLACEMENT_3D('',#9029,#7199,#7200);
#6145=AXIS2_PLACEMENT_3D('',#9030,#7201,#7202);
#6146=AXIS2_PLACEMENT_3D('',#9032,#7203,#7204);
#6147=AXIS2_PLACEMENT_3D('',#9034,#7206,#7207);
#6148=AXIS2_PLACEMENT_3D('',#9036,#7208,#7209);
#6149=AXIS2_PLACEMENT_3D('',#9038,#7211,#7212);
#6150=AXIS2_PLACEMENT_3D('',#9040,#7213,#7214);
#6151=AXIS2_PLACEMENT_3D('',#9042,#7216,#7217);
#6152=AXIS2_PLACEMENT_3D('',#9044,#7218,#7219);
#6153=AXIS2_PLACEMENT_3D('',#9046,#7221,#7222);
#6154=AXIS2_PLACEMENT_3D('',#9048,#7223,#7224);
#6155=AXIS2_PLACEMENT_3D('',#9051,#7226,#7227);
#6156=AXIS2_PLACEMENT_3D('',#9052,#7228,#7229);
#6157=AXIS2_PLACEMENT_3D('',#9054,#7230,#7231);
#6158=AXIS2_PLACEMENT_3D('',#9055,#7232,#7233);
#6159=AXIS2_PLACEMENT_3D('',#9057,#7235,#7236);
#6160=AXIS2_PLACEMENT_3D('',#9060,#7238,#7239);
#6161=AXIS2_PLACEMENT_3D('',#9061,#7240,#7241);
#6162=AXIS2_PLACEMENT_3D('',#9062,#7242,#7243);
#6163=AXIS2_PLACEMENT_3D('',#9063,#7244,#7245);
#6164=AXIS2_PLACEMENT_3D('',#9065,#7246,#7247);
#6165=AXIS2_PLACEMENT_3D('',#9066,#7248,#7249);
#6166=AXIS2_PLACEMENT_3D('',#9068,#7250,#7251);
#6167=AXIS2_PLACEMENT_3D('',#9070,#7253,#7254);
#6168=AXIS2_PLACEMENT_3D('',#9072,#7255,#7256);
#6169=AXIS2_PLACEMENT_3D('',#9074,#7258,#7259);
#6170=AXIS2_PLACEMENT_3D('',#9076,#7260,#7261);
#6171=AXIS2_PLACEMENT_3D('',#9078,#7263,#7264);
#6172=AXIS2_PLACEMENT_3D('',#9080,#7265,#7266);
#6173=AXIS2_PLACEMENT_3D('',#9081,#7267,#7268);
#6174=AXIS2_PLACEMENT_3D('',#9083,#7269,#7270);
#6175=AXIS2_PLACEMENT_3D('',#9085,#7272,#7273);
#6176=AXIS2_PLACEMENT_3D('',#9087,#7274,#7275);
#6177=AXIS2_PLACEMENT_3D('',#9089,#7277,#7278);
#6178=AXIS2_PLACEMENT_3D('',#9091,#7279,#7280);
#6179=AXIS2_PLACEMENT_3D('',#9093,#7282,#7283);
#6180=AXIS2_PLACEMENT_3D('',#9094,#7284,#7285);
#6181=AXIS2_PLACEMENT_3D('',#9103,#7290,#7291);
#6182=AXIS2_PLACEMENT_3D('',#9109,#7295,#7296);
#6183=AXIS2_PLACEMENT_3D('',#9115,#7300,#7301);
#6184=AXIS2_PLACEMENT_3D('',#9121,#7305,#7306);
#6185=AXIS2_PLACEMENT_3D('',#9127,#7310,#7311);
#6186=AXIS2_PLACEMENT_3D('',#9130,#7314,#7315);
#6187=AXIS2_PLACEMENT_3D('',#9131,#7316,#7317);
#6188=AXIS2_PLACEMENT_3D('',#9132,#7318,#7319);
#6189=AXIS2_PLACEMENT_3D('',#9133,#7320,#7321);
#6190=AXIS2_PLACEMENT_3D('',#9134,#7322,#7323);
#6191=AXIS2_PLACEMENT_3D('',#9137,#7324,#7325);
#6192=AXIS2_PLACEMENT_3D('',#9138,#7326,#7327);
#6193=AXIS2_PLACEMENT_3D('',#9140,#7328,#7329);
#6194=AXIS2_PLACEMENT_3D('',#9142,#7330,#7331);
#6195=AXIS2_PLACEMENT_3D('',#9143,#7332,#7333);
#6196=AXIS2_PLACEMENT_3D('',#9144,#7334,#7335);
#6197=AXIS2_PLACEMENT_3D('',#9147,#7337,#7338);
#6198=AXIS2_PLACEMENT_3D('',#9148,#7339,#7340);
#6199=AXIS2_PLACEMENT_3D('',#9150,#7341,#7342);
#6200=AXIS2_PLACEMENT_3D('',#9153,#7344,#7345);
#6201=AXIS2_PLACEMENT_3D('',#9154,#7346,#7347);
#6202=AXIS2_PLACEMENT_3D('',#9157,#7349,#7350);
#6203=AXIS2_PLACEMENT_3D('',#9158,#7351,#7352);
#6204=AXIS2_PLACEMENT_3D('',#9159,#7353,#7354);
#6205=AXIS2_PLACEMENT_3D('',#9161,#7355,#7356);
#6206=AXIS2_PLACEMENT_3D('',#9163,#7358,#7359);
#6207=AXIS2_PLACEMENT_3D('',#9165,#7360,#7361);
#6208=AXIS2_PLACEMENT_3D('',#9166,#7362,#7363);
#6209=AXIS2_PLACEMENT_3D('',#9168,#7365,#7366);
#6210=AXIS2_PLACEMENT_3D('',#9169,#7367,#7368);
#6211=AXIS2_PLACEMENT_3D('',#9172,#7369,#7370);
#6212=AXIS2_PLACEMENT_3D('',#9173,#7371,#7372);
#6213=AXIS2_PLACEMENT_3D('',#9175,#7373,#7374);
#6214=AXIS2_PLACEMENT_3D('',#9177,#7375,#7376);
#6215=AXIS2_PLACEMENT_3D('',#9178,#7377,#7378);
#6216=AXIS2_PLACEMENT_3D('',#9179,#7379,#7380);
#6217=AXIS2_PLACEMENT_3D('',#9181,#7381,#7382);
#6218=AXIS2_PLACEMENT_3D('',#9183,#7384,#7385);
#6219=AXIS2_PLACEMENT_3D('',#9185,#7386,#7387);
#6220=AXIS2_PLACEMENT_3D('',#9187,#7388,#7389);
#6221=AXIS2_PLACEMENT_3D('',#9188,#7390,#7391);
#6222=AXIS2_PLACEMENT_3D('',#9190,#7392,#7393);
#6223=AXIS2_PLACEMENT_3D('',#9192,#7395,#7396);
#6224=AXIS2_PLACEMENT_3D('',#9194,#7397,#7398);
#6225=AXIS2_PLACEMENT_3D('',#9196,#7400,#7401);
#6226=AXIS2_PLACEMENT_3D('',#9198,#7402,#7403);
#6227=AXIS2_PLACEMENT_3D('',#9200,#7405,#7406);
#6228=AXIS2_PLACEMENT_3D('',#9201,#7407,#7408);
#6229=AXIS2_PLACEMENT_3D('',#9203,#7410,#7411);
#6230=AXIS2_PLACEMENT_3D('',#9204,#7412,#7413);
#6231=AXIS2_PLACEMENT_3D('',#9207,#7414,#7415);
#6232=AXIS2_PLACEMENT_3D('',#9208,#7416,#7417);
#6233=AXIS2_PLACEMENT_3D('',#9211,#7418,#7419);
#6234=AXIS2_PLACEMENT_3D('',#9212,#7420,#7421);
#6235=AXIS2_PLACEMENT_3D('',#9215,#7422,#7423);
#6236=AXIS2_PLACEMENT_3D('',#9216,#7424,#7425);
#6237=AXIS2_PLACEMENT_3D('',#9219,#7426,#7427);
#6238=AXIS2_PLACEMENT_3D('',#9220,#7428,#7429);
#6239=AXIS2_PLACEMENT_3D('',#9223,#7430,#7431);
#6240=AXIS2_PLACEMENT_3D('',#9224,#7432,#7433);
#6241=AXIS2_PLACEMENT_3D('',#9227,#7434,#7435);
#6242=AXIS2_PLACEMENT_3D('',#9228,#7436,#7437);
#6243=AXIS2_PLACEMENT_3D('',#9231,#7438,#7439);
#6244=AXIS2_PLACEMENT_3D('',#9232,#7440,#7441);
#6245=AXIS2_PLACEMENT_3D('',#9235,#7442,#7443);
#6246=AXIS2_PLACEMENT_3D('',#9236,#7444,#7445);
#6247=AXIS2_PLACEMENT_3D('',#9237,#7446,#7447);
#6248=AXIS2_PLACEMENT_3D('',#9263,#7448,#7449);
#6249=AXIS2_PLACEMENT_3D('',#9287,#7450,#7451);
#6250=AXIS2_PLACEMENT_3D('',#9288,#7452,#7453);
#6251=AXIS2_PLACEMENT_3D('',#9290,#7454,#7455);
#6252=AXIS2_PLACEMENT_3D('',#9315,#7456,#7457);
#6253=AXIS2_PLACEMENT_3D('',#9340,#7458,#7459);
#6254=AXIS2_PLACEMENT_3D('',#9356,#7461,#7462);
#6255=AXIS2_PLACEMENT_3D('',#9371,#7463,#7464);
#6256=AXIS2_PLACEMENT_3D('',#9396,#7465,#7466);
#6257=AXIS2_PLACEMENT_3D('',#9421,#7467,#7468);
#6258=AXIS2_PLACEMENT_3D('',#9446,#7469,#7470);
#6259=AXIS2_PLACEMENT_3D('',#9470,#7471,#7472);
#6260=AXIS2_PLACEMENT_3D('',#9471,#7473,#7474);
#6261=AXIS2_PLACEMENT_3D('',#9473,#7475,#7476);
#6262=AXIS2_PLACEMENT_3D('',#9474,#7477,#7478);
#6263=AXIS2_PLACEMENT_3D('',#9475,#7479,#7480);
#6264=AXIS2_PLACEMENT_3D('',#9499,#7481,#7482);
#6265=AXIS2_PLACEMENT_3D('',#9500,#7483,#7484);
#6266=AXIS2_PLACEMENT_3D('',#9502,#7485,#7486);
#6267=AXIS2_PLACEMENT_3D('',#9503,#7487,#7488);
#6268=AXIS2_PLACEMENT_3D('',#9504,#7489,#7490);
#6269=AXIS2_PLACEMENT_3D('',#9528,#7491,#7492);
#6270=AXIS2_PLACEMENT_3D('',#9529,#7493,#7494);
#6271=AXIS2_PLACEMENT_3D('',#9531,#7495,#7496);
#6272=AXIS2_PLACEMENT_3D('',#9532,#7497,#7498);
#6273=AXIS2_PLACEMENT_3D('',#9533,#7499,#7500);
#6274=AXIS2_PLACEMENT_3D('',#9548,#7501,#7502);
#6275=AXIS2_PLACEMENT_3D('',#9561,#7503,#7504);
#6276=AXIS2_PLACEMENT_3D('',#9563,#7505,#7506);
#6277=AXIS2_PLACEMENT_3D('',#9564,#7507,#7508);
#6278=AXIS2_PLACEMENT_3D('',#9565,#7509,#7510);
#6279=AXIS2_PLACEMENT_3D('',#9589,#7511,#7512);
#6280=AXIS2_PLACEMENT_3D('',#9590,#7513,#7514);
#6281=AXIS2_PLACEMENT_3D('',#9592,#7515,#7516);
#6282=AXIS2_PLACEMENT_3D('',#9593,#7517,#7518);
#6283=AXIS2_PLACEMENT_3D('',#9594,#7519,#7520);
#6284=AXIS2_PLACEMENT_3D('',#9618,#7521,#7522);
#6285=AXIS2_PLACEMENT_3D('',#9619,#7523,#7524);
#6286=AXIS2_PLACEMENT_3D('',#9621,#7525,#7526);
#6287=AXIS2_PLACEMENT_3D('',#9622,#7527,#7528);
#6288=AXIS2_PLACEMENT_3D('',#9623,#7529,#7530);
#6289=AXIS2_PLACEMENT_3D('',#9647,#7531,#7532);
#6290=AXIS2_PLACEMENT_3D('',#9648,#7533,#7534);
#6291=AXIS2_PLACEMENT_3D('',#9650,#7535,#7536);
#6292=AXIS2_PLACEMENT_3D('',#9653,#7538,#7539);
#6293=AXIS2_PLACEMENT_3D('',#9677,#7540,#7541);
#6294=AXIS2_PLACEMENT_3D('',#9678,#7542,#7543);
#6295=AXIS2_PLACEMENT_3D('',#9679,#7544,#7545);
#6296=AXIS2_PLACEMENT_3D('',#9680,#7546,#7547);
#6297=AXIS2_PLACEMENT_3D('',#9681,#7548,#7549);
#6298=AXIS2_PLACEMENT_3D('',#9682,#7550,#7551);
#6299=AXIS2_PLACEMENT_3D('',#9683,#7552,#7553);
#6300=AXIS2_PLACEMENT_3D('',#9684,#7554,#7555);
#6301=AXIS2_PLACEMENT_3D('',#9685,#7556,#7557);
#6302=AXIS2_PLACEMENT_3D('',#9687,#7558,#7559);
#6303=AXIS2_PLACEMENT_3D('',#9689,#7560,#7561);
#6304=AXIS2_PLACEMENT_3D('',#9690,#7562,#7563);
#6305=AXIS2_PLACEMENT_3D('',#9692,#7564,#7565);
#6306=AXIS2_PLACEMENT_3D('',#9694,#7567,#7568);
#6307=AXIS2_PLACEMENT_3D('',#9696,#7569,#7570);
#6308=AXIS2_PLACEMENT_3D('',#9697,#7571,#7572);
#6309=AXIS2_PLACEMENT_3D('',#9699,#7574,#7575);
#6310=AXIS2_PLACEMENT_3D('',#9701,#7576,#7577);
#6311=AXIS2_PLACEMENT_3D('',#9703,#7578,#7579);
#6312=AXIS2_PLACEMENT_3D('',#9704,#7580,#7581);
#6313=AXIS2_PLACEMENT_3D('',#9706,#7582,#7583);
#6314=AXIS2_PLACEMENT_3D('',#9708,#7585,#7586);
#6315=AXIS2_PLACEMENT_3D('',#9710,#7587,#7588);
#6316=AXIS2_PLACEMENT_3D('',#9711,#7589,#7590);
#6317=AXIS2_PLACEMENT_3D('',#9713,#7592,#7593);
#6318=AXIS2_PLACEMENT_3D('',#9714,#7594,#7595);
#6319=AXIS2_PLACEMENT_3D('',#9715,#7596,#7597);
#6320=AXIS2_PLACEMENT_3D('',#9716,#7598,#7599);
#6321=AXIS2_PLACEMENT_3D('',#9717,#7600,#7601);
#6322=AXIS2_PLACEMENT_3D('',#9718,#7602,#7603);
#6323=AXIS2_PLACEMENT_3D('',#9719,#7604,#7605);
#6324=AXIS2_PLACEMENT_3D('',#9720,#7606,#7607);
#6325=AXIS2_PLACEMENT_3D('',#9722,#7608,#7609);
#6326=AXIS2_PLACEMENT_3D('',#9725,#7611,#7612);
#6327=AXIS2_PLACEMENT_3D('',#9726,#7613,#7614);
#6328=AXIS2_PLACEMENT_3D('',#9727,#7615,#7616);
#6329=AXIS2_PLACEMENT_3D('',#9729,#7617,#7618);
#6330=AXIS2_PLACEMENT_3D('',#9732,#7620,#7621);
#6331=AXIS2_PLACEMENT_3D('',#9733,#7622,#7623);
#6332=AXIS2_PLACEMENT_3D('',#9738,#7625,#7626);
#6333=AXIS2_PLACEMENT_3D('',#9741,#7628,#7629);
#6334=AXIS2_PLACEMENT_3D('',#9742,#7630,#7631);
#6335=AXIS2_PLACEMENT_3D('',#9746,#7633,#7634);
#6336=AXIS2_PLACEMENT_3D('',#9754,#7638,#7639);
#6337=AXIS2_PLACEMENT_3D('',#9757,#7641,#7642);
#6338=AXIS2_PLACEMENT_3D('',#9758,#7643,#7644);
#6339=AXIS2_PLACEMENT_3D('',#9762,#7647,#7648);
#6340=AXIS2_PLACEMENT_3D('',#9766,#7651,#7652);
#6341=AXIS2_PLACEMENT_3D('',#9772,#7656,#7657);
#6342=AXIS2_PLACEMENT_3D('',#9778,#7661,#7662);
#6343=AXIS2_PLACEMENT_3D('',#9780,#7664,#7665);
#6344=AXIS2_PLACEMENT_3D('',#9781,#7666,#7667);
#6345=AXIS2_PLACEMENT_3D('',#9782,#7668,#7669);
#6346=AXIS2_PLACEMENT_3D('',#9784,#7670,#7671);
#6347=AXIS2_PLACEMENT_3D('',#9785,#7672,#7673);
#6348=AXIS2_PLACEMENT_3D('',#9786,#7674,#7675);
#6349=AXIS2_PLACEMENT_3D('',#9787,#7676,#7677);
#6350=AXIS2_PLACEMENT_3D('',#9789,#7678,#7679);
#6351=AXIS2_PLACEMENT_3D('',#9791,#7680,#7681);
#6352=AXIS2_PLACEMENT_3D('',#9792,#7682,#7683);
#6353=AXIS2_PLACEMENT_3D('',#9794,#7685,#7686);
#6354=AXIS2_PLACEMENT_3D('',#9797,#7688,#7689);
#6355=AXIS2_PLACEMENT_3D('',#9798,#7690,#7691);
#6356=AXIS2_PLACEMENT_3D('',#9800,#7692,#7693);
#6357=AXIS2_PLACEMENT_3D('',#9802,#7695,#7696);
#6358=AXIS2_PLACEMENT_3D('',#9803,#7697,#7698);
#6359=AXIS2_PLACEMENT_3D('',#9804,#7699,#7700);
#6360=AXIS2_PLACEMENT_3D('',#9805,#7701,#7702);
#6361=AXIS2_PLACEMENT_3D('',#9807,#7703,#7704);
#6362=AXIS2_PLACEMENT_3D('',#9810,#7706,#7707);
#6363=AXIS2_PLACEMENT_3D('',#9811,#7708,#7709);
#6364=AXIS2_PLACEMENT_3D('',#9813,#7710,#7711);
#6365=AXIS2_PLACEMENT_3D('',#9816,#7713,#7714);
#6366=AXIS2_PLACEMENT_3D('',#9817,#7715,#7716);
#6367=AXIS2_PLACEMENT_3D('',#9818,#7717,#7718);
#6368=AXIS2_PLACEMENT_3D('',#9819,#7719,#7720);
#6369=AXIS2_PLACEMENT_3D('',#9820,#7721,#7722);
#6370=AXIS2_PLACEMENT_3D('',#9825,#7724,#7725);
#6371=AXIS2_PLACEMENT_3D('',#9826,#7726,#7727);
#6372=AXIS2_PLACEMENT_3D('',#9827,#7728,#7729);
#6373=AXIS2_PLACEMENT_3D('',#9880,#7731,#7732);
#6374=AXIS2_PLACEMENT_3D('',#9895,#7733,#7734);
#6375=AXIS2_PLACEMENT_3D('',#9897,#7736,#7737);
#6376=AXIS2_PLACEMENT_3D('',#9901,#7739,#7740);
#6377=AXIS2_PLACEMENT_3D('',#9902,#7741,#7742);
#6378=AXIS2_PLACEMENT_3D('',#9956,#7744,#7745);
#6379=AXIS2_PLACEMENT_3D('',#9982,#7746,#7747);
#6380=AXIS2_PLACEMENT_3D('',#9984,#7749,#7750);
#6381=AXIS2_PLACEMENT_3D('',#9986,#7751,#7752);
#6382=AXIS2_PLACEMENT_3D('',#9990,#7755,#7756);
#6383=AXIS2_PLACEMENT_3D('',#9991,#7757,#7758);
#6384=AXIS2_PLACEMENT_3D('',#9993,#7759,#7760);
#6385=AXIS2_PLACEMENT_3D('',#9997,#7763,#7764);
#6386=AXIS2_PLACEMENT_3D('',#9998,#7765,#7766);
#6387=AXIS2_PLACEMENT_3D('',#9999,#7767,#7768);
#6388=AXIS2_PLACEMENT_3D('',#10000,#7769,#7770);
#6389=AXIS2_PLACEMENT_3D('',#10001,#7771,#7772);
#6390=AXIS2_PLACEMENT_3D('',#10003,#7773,#7774);
#6391=AXIS2_PLACEMENT_3D('',#10005,#7775,#7776);
#6392=AXIS2_PLACEMENT_3D('',#10006,#7777,#7778);
#6393=AXIS2_PLACEMENT_3D('',#10008,#7779,#7780);
#6394=AXIS2_PLACEMENT_3D('',#10010,#7781,#7782);
#6395=AXIS2_PLACEMENT_3D('',#10011,#7783,#7784);
#6396=AXIS2_PLACEMENT_3D('',#10013,#7786,#7787);
#6397=AXIS2_PLACEMENT_3D('',#10016,#7789,#7790);
#6398=AXIS2_PLACEMENT_3D('',#10017,#7791,#7792);
#6399=AXIS2_PLACEMENT_3D('',#10019,#7793,#7794);
#6400=AXIS2_PLACEMENT_3D('',#10021,#7796,#7797);
#6401=AXIS2_PLACEMENT_3D('',#10022,#7798,#7799);
#6402=AXIS2_PLACEMENT_3D('',#10023,#7800,#7801);
#6403=AXIS2_PLACEMENT_3D('',#10024,#7802,#7803);
#6404=AXIS2_PLACEMENT_3D('',#10026,#7804,#7805);
#6405=AXIS2_PLACEMENT_3D('',#10029,#7807,#7808);
#6406=AXIS2_PLACEMENT_3D('',#10030,#7809,#7810);
#6407=AXIS2_PLACEMENT_3D('',#10035,#7812,#7813);
#6408=AXIS2_PLACEMENT_3D('',#10038,#7815,#7816);
#6409=AXIS2_PLACEMENT_3D('',#10039,#7817,#7818);
#6410=AXIS2_PLACEMENT_3D('',#10043,#7820,#7821);
#6411=AXIS2_PLACEMENT_3D('',#10045,#7823,#7824);
#6412=AXIS2_PLACEMENT_3D('',#10049,#7827,#7828);
#6413=AXIS2_PLACEMENT_3D('',#10053,#7831,#7832);
#6414=AXIS2_PLACEMENT_3D('',#10054,#7833,#7834);
#6415=AXIS2_PLACEMENT_3D('',#10055,#7835,#7836);
#6416=AXIS2_PLACEMENT_3D('',#10056,#7837,#7838);
#6417=AXIS2_PLACEMENT_3D('',#10057,#7839,#7840);
#6418=AXIS2_PLACEMENT_3D('',#10059,#7841,#7842);
#6419=AXIS2_PLACEMENT_3D('',#10062,#7844,#7845);
#6420=AXIS2_PLACEMENT_3D('',#10063,#7846,#7847);
#6421=AXIS2_PLACEMENT_3D('',#10065,#7848,#7849);
#6422=AXIS2_PLACEMENT_3D('',#10068,#7851,#7852);
#6423=AXIS2_PLACEMENT_3D('',#10069,#7853,#7854);
#6424=AXIS2_PLACEMENT_3D('',#10070,#7855,#7856);
#6425=AXIS2_PLACEMENT_3D('',#10071,#7857,#7858);
#6426=AXIS2_PLACEMENT_3D('',#10072,#7859,#7860);
#6427=AXIS2_PLACEMENT_3D('',#10074,#7861,#7862);
#6428=AXIS2_PLACEMENT_3D('',#10077,#7864,#7865);
#6429=AXIS2_PLACEMENT_3D('',#10078,#7866,#7867);
#6430=AXIS2_PLACEMENT_3D('',#10080,#7868,#7869);
#6431=AXIS2_PLACEMENT_3D('',#10083,#7871,#7872);
#6432=AXIS2_PLACEMENT_3D('',#10084,#7873,#7874);
#6433=AXIS2_PLACEMENT_3D('',#10085,#7875,#7876);
#6434=AXIS2_PLACEMENT_3D('',#10086,#7877,#7878);
#6435=AXIS2_PLACEMENT_3D('',#10087,#7879,#7880);
#6436=AXIS2_PLACEMENT_3D('',#10089,#7881,#7882);
#6437=AXIS2_PLACEMENT_3D('',#10092,#7884,#7885);
#6438=AXIS2_PLACEMENT_3D('',#10093,#7886,#7887);
#6439=AXIS2_PLACEMENT_3D('',#10095,#7888,#7889);
#6440=AXIS2_PLACEMENT_3D('',#10098,#7891,#7892);
#6441=AXIS2_PLACEMENT_3D('',#10099,#7893,#7894);
#6442=AXIS2_PLACEMENT_3D('',#10100,#7895,#7896);
#6443=AXIS2_PLACEMENT_3D('',#10101,#7897,#7898);
#6444=AXIS2_PLACEMENT_3D('',#10102,#7899,#7900);
#6445=AXIS2_PLACEMENT_3D('',#10111,#7905,#7906);
#6446=AXIS2_PLACEMENT_3D('',#10117,#7910,#7911);
#6447=AXIS2_PLACEMENT_3D('',#10123,#7915,#7916);
#6448=AXIS2_PLACEMENT_3D('',#10129,#7920,#7921);
#6449=AXIS2_PLACEMENT_3D('',#10135,#7925,#7926);
#6450=AXIS2_PLACEMENT_3D('',#10138,#7929,#7930);
#6451=AXIS2_PLACEMENT_3D('',#10139,#7931,#7932);
#6452=AXIS2_PLACEMENT_3D('',#10140,#7933,#7934);
#6453=AXIS2_PLACEMENT_3D('',#10142,#7935,#7936);
#6454=AXIS2_PLACEMENT_3D('',#10143,#7937,#7938);
#6455=AXIS2_PLACEMENT_3D('',#10145,#7939,#7940);
#6456=AXIS2_PLACEMENT_3D('',#10146,#7941,#7942);
#6457=AXIS2_PLACEMENT_3D('',#10148,#7943,#7944);
#6458=AXIS2_PLACEMENT_3D('',#10150,#7946,#7947);
#6459=AXIS2_PLACEMENT_3D('',#10152,#7948,#7949);
#6460=AXIS2_PLACEMENT_3D('',#10154,#7951,#7952);
#6461=AXIS2_PLACEMENT_3D('',#10156,#7953,#7954);
#6462=AXIS2_PLACEMENT_3D('',#10158,#7956,#7957);
#6463=AXIS2_PLACEMENT_3D('',#10160,#7958,#7959);
#6464=AXIS2_PLACEMENT_3D('',#10161,#7960,#7961);
#6465=AXIS2_PLACEMENT_3D('',#10163,#7962,#7963);
#6466=AXIS2_PLACEMENT_3D('',#10165,#7965,#7966);
#6467=AXIS2_PLACEMENT_3D('',#10167,#7968,#7969);
#6468=AXIS2_PLACEMENT_3D('',#10168,#7970,#7971);
#6469=AXIS2_PLACEMENT_3D('',#10169,#7972,#7973);
#6470=AXIS2_PLACEMENT_3D('',#10170,#7974,#7975);
#6471=AXIS2_PLACEMENT_3D('',#10171,#7976,#7977);
#6472=AXIS2_PLACEMENT_3D('',#10172,#7978,#7979);
#6473=AXIS2_PLACEMENT_3D('',#10173,#7980,#7981);
#6474=AXIS2_PLACEMENT_3D('',#10174,#7982,#7983);
#6475=AXIS2_PLACEMENT_3D('',#10175,#7984,#7985);
#6476=AXIS2_PLACEMENT_3D('',#10176,#7986,#7987);
#6477=AXIS2_PLACEMENT_3D('',#10177,#7988,#7989);
#6478=AXIS2_PLACEMENT_3D('',#10178,#7990,#7991);
#6479=AXIS2_PLACEMENT_3D('',#10179,#7992,#7993);
#6480=AXIS2_PLACEMENT_3D('',#10180,#7994,#7995);
#6481=AXIS2_PLACEMENT_3D('',#10181,#7996,#7997);
#6482=AXIS2_PLACEMENT_3D('',#10182,#7998,#7999);
#6483=AXIS2_PLACEMENT_3D('',#10183,#8000,#8001);
#6484=AXIS2_PLACEMENT_3D('',#10184,#8002,#8003);
#6485=AXIS2_PLACEMENT_3D('',#10185,#8004,#8005);
#6486=AXIS2_PLACEMENT_3D('',#10186,#8006,#8007);
#6487=AXIS2_PLACEMENT_3D('',#10187,#8008,#8009);
#6488=AXIS2_PLACEMENT_3D('',#10188,#8010,#8011);
#6489=AXIS2_PLACEMENT_3D('',#10190,#8012,#8013);
#6490=AXIS2_PLACEMENT_3D('',#10193,#8015,#8016);
#6491=AXIS2_PLACEMENT_3D('',#10194,#8017,#8018);
#6492=AXIS2_PLACEMENT_3D('',#10196,#8019,#8020);
#6493=AXIS2_PLACEMENT_3D('',#10199,#8022,#8023);
#6494=AXIS2_PLACEMENT_3D('',#10200,#8024,#8025);
#6495=AXIS2_PLACEMENT_3D('',#10202,#8026,#8027);
#6496=AXIS2_PLACEMENT_3D('',#10205,#8029,#8030);
#6497=AXIS2_PLACEMENT_3D('',#10206,#8031,#8032);
#6498=AXIS2_PLACEMENT_3D('',#10208,#8033,#8034);
#6499=AXIS2_PLACEMENT_3D('',#10211,#8036,#8037);
#6500=AXIS2_PLACEMENT_3D('',#10212,#8038,#8039);
#6501=AXIS2_PLACEMENT_3D('',#10215,#8040,#8041);
#6502=AXIS2_PLACEMENT_3D('',#10219,#8043,#8044);
#6503=AXIS2_PLACEMENT_3D('',#10221,#8046,#8047);
#6504=AXIS2_PLACEMENT_3D('',#10224,#8048,#8049);
#6505=AXIS2_PLACEMENT_3D('',#10228,#8051,#8052);
#6506=AXIS2_PLACEMENT_3D('',#10230,#8054,#8055);
#6507=AXIS2_PLACEMENT_3D('',#10233,#8056,#8057);
#6508=AXIS2_PLACEMENT_3D('',#10237,#8059,#8060);
#6509=AXIS2_PLACEMENT_3D('',#10239,#8062,#8063);
#6510=AXIS2_PLACEMENT_3D('',#10244,#8065,#8066);
#6511=AXIS2_PLACEMENT_3D('',#10247,#8068,#8069);
#6512=AXIS2_PLACEMENT_3D('',#10248,#8070,#8071);
#6513=AXIS2_PLACEMENT_3D('',#10250,#8072,#8073);
#6514=AXIS2_PLACEMENT_3D('',#10253,#8075,#8076);
#6515=AXIS2_PLACEMENT_3D('',#10254,#8077,#8078);
#6516=AXIS2_PLACEMENT_3D('',#10256,#8079,#8080);
#6517=AXIS2_PLACEMENT_3D('',#10259,#8082,#8083);
#6518=AXIS2_PLACEMENT_3D('',#10260,#8084,#8085);
#6519=AXIS2_PLACEMENT_3D('',#10262,#8086,#8087);
#6520=AXIS2_PLACEMENT_3D('',#10265,#8089,#8090);
#6521=AXIS2_PLACEMENT_3D('',#10266,#8091,#8092);
#6522=AXIS2_PLACEMENT_3D('',#10274,#8096,#8097);
#6523=AXIS2_PLACEMENT_3D('',#10281,#8101,#8102);
#6524=AXIS2_PLACEMENT_3D('',#10283,#8103,#8104);
#6525=AXIS2_PLACEMENT_3D('',#10291,#8108,#8109);
#6526=AXIS2_PLACEMENT_3D('',#10298,#8113,#8114);
#6527=AXIS2_PLACEMENT_3D('',#10306,#8118,#8119);
#6528=AXIS2_PLACEMENT_3D('',#10313,#8123,#8124);
#6529=AXIS2_PLACEMENT_3D('',#10321,#8128,#8129);
#6530=AXIS2_PLACEMENT_3D('',#10328,#8133,#8134);
#6531=AXIS2_PLACEMENT_3D('',#10329,#8135,#8136);
#6532=AXIS2_PLACEMENT_3D('',#10331,#8137,#8138);
#6533=AXIS2_PLACEMENT_3D('',#10333,#8140,#8141);
#6534=AXIS2_PLACEMENT_3D('',#10336,#8143,#8144);
#6535=AXIS2_PLACEMENT_3D('',#10337,#8145,#8146);
#6536=AXIS2_PLACEMENT_3D('',#10341,#8149,#8150);
#6537=AXIS2_PLACEMENT_3D('',#10345,#8153,#8154);
#6538=AXIS2_PLACEMENT_3D('',#10351,#8158,#8159);
#6539=AXIS2_PLACEMENT_3D('',#10353,#8161,#8162);
#6540=AXIS2_PLACEMENT_3D('',#10357,#8165,#8166);
#6541=AXIS2_PLACEMENT_3D('',#10359,#8167,#8168);
#6542=AXIS2_PLACEMENT_3D('',#10367,#8172,#8173);
#6543=AXIS2_PLACEMENT_3D('',#10369,#8174,#8175);
#6544=AXIS2_PLACEMENT_3D('',#10370,#8176,#8177);
#6545=AXIS2_PLACEMENT_3D('',#10371,#8178,#8179);
#6546=AXIS2_PLACEMENT_3D('',#10375,#8181,#8182);
#6547=AXIS2_PLACEMENT_3D('',#10377,#8183,#8184);
#6548=AXIS2_PLACEMENT_3D('',#10379,#8185,#8186);
#6549=AXIS2_PLACEMENT_3D('',#10385,#8190,#8191);
#6550=AXIS2_PLACEMENT_3D('',#10388,#8192,#8193);
#6551=AXIS2_PLACEMENT_3D('',#10389,#8194,#8195);
#6552=AXIS2_PLACEMENT_3D('',#10390,#8196,#8197);
#6553=AXIS2_PLACEMENT_3D('',#10394,#8201,#8202);
#6554=AXIS2_PLACEMENT_3D('',#10398,#8204,#8205);
#6555=AXIS2_PLACEMENT_3D('',#10401,#8207,#8208);
#6556=AXIS2_PLACEMENT_3D('',#10403,#8209,#8210);
#6557=AXIS2_PLACEMENT_3D('',#10407,#8212,#8213);
#6558=AXIS2_PLACEMENT_3D('',#10411,#8215,#8216);
#6559=AXIS2_PLACEMENT_3D('',#10415,#8218,#8219);
#6560=AXIS2_PLACEMENT_3D('',#10419,#8221,#8222);
#6561=AXIS2_PLACEMENT_3D('',#10421,#8224,#8225);
#6562=AXIS2_PLACEMENT_3D('',#10422,#8226,#8227);
#6563=AXIS2_PLACEMENT_3D('',#10424,#8229,#8230);
#6564=AXIS2_PLACEMENT_3D('',#10426,#8232,#8233);
#6565=AXIS2_PLACEMENT_3D('',#10428,#8235,#8236);
#6566=AXIS2_PLACEMENT_3D('',#10434,#8240,#8241);
#6567=AXIS2_PLACEMENT_3D('',#10436,#8243,#8244);
#6568=AXIS2_PLACEMENT_3D('',#10440,#8247,#8248);
#6569=AXIS2_PLACEMENT_3D('',#10442,#8249,#8250);
#6570=AXIS2_PLACEMENT_3D('',#10449,#8254,#8255);
#6571=AXIS2_PLACEMENT_3D('',#10450,#8256,#8257);
#6572=AXIS2_PLACEMENT_3D('',#10451,#8258,#8259);
#6573=AXIS2_PLACEMENT_3D('',#10452,#8260,#8261);
#6574=AXIS2_PLACEMENT_3D('',#10453,#8262,#8263);
#6575=AXIS2_PLACEMENT_3D('',#10455,#8265,#8266);
#6576=AXIS2_PLACEMENT_3D('',#10456,#8267,#8268);
#6577=AXIS2_PLACEMENT_3D('',#10458,#8270,#8271);
#6578=AXIS2_PLACEMENT_3D('',#10460,#8273,#8274);
#6579=AXIS2_PLACEMENT_3D('',#10462,#8276,#8277);
#6580=AXIS2_PLACEMENT_3D('',#10468,#8281,#8282);
#6581=AXIS2_PLACEMENT_3D('',#10470,#8284,#8285);
#6582=AXIS2_PLACEMENT_3D('',#10474,#8288,#8289);
#6583=AXIS2_PLACEMENT_3D('',#10476,#8290,#8291);
#6584=AXIS2_PLACEMENT_3D('',#10483,#8295,#8296);
#6585=AXIS2_PLACEMENT_3D('',#10484,#8297,#8298);
#6586=AXIS2_PLACEMENT_3D('',#10485,#8299,#8300);
#6587=AXIS2_PLACEMENT_3D('',#10486,#8301,#8302);
#6588=AXIS2_PLACEMENT_3D('',#10487,#8303,#8304);
#6589=AXIS2_PLACEMENT_3D('',#10489,#8306,#8307);
#6590=AXIS2_PLACEMENT_3D('',#10490,#8308,#8309);
#6591=AXIS2_PLACEMENT_3D('',#10492,#8311,#8312);
#6592=AXIS2_PLACEMENT_3D('',#10494,#8314,#8315);
#6593=AXIS2_PLACEMENT_3D('',#10496,#8317,#8318);
#6594=AXIS2_PLACEMENT_3D('',#10498,#8320,#8321);
#6595=AXIS2_PLACEMENT_3D('',#10500,#8323,#8324);
#6596=AXIS2_PLACEMENT_3D('',#10501,#8325,#8326);
#6597=AXIS2_PLACEMENT_3D('',#10502,#8327,#8328);
#6598=AXIS2_PLACEMENT_3D('',#10505,#8331,#8332);
#6599=AXIS2_PLACEMENT_3D('',#10506,#8333,#8334);
#6600=AXIS2_PLACEMENT_3D('',#10507,#8335,#8336);
#6601=AXIS2_PLACEMENT_3D('',#10509,#8337,#8338);
#6602=AXIS2_PLACEMENT_3D('',#10510,#8339,#8340);
#6603=AXIS2_PLACEMENT_3D('',#10513,#8342,#8343);
#6604=AXIS2_PLACEMENT_3D('',#10514,#8344,#8345);
#6605=AXIS2_PLACEMENT_3D('',#10515,#8346,#8347);
#6606=AXIS2_PLACEMENT_3D('',#10516,#8348,#8349);
#6607=AXIS2_PLACEMENT_3D('',#10518,#8350,#8351);
#6608=AXIS2_PLACEMENT_3D('',#10521,#8353,#8354);
#6609=AXIS2_PLACEMENT_3D('',#10522,#8355,#8356);
#6610=AXIS2_PLACEMENT_3D('',#10524,#8357,#8358);
#6611=AXIS2_PLACEMENT_3D('',#10527,#8360,#8361);
#6612=AXIS2_PLACEMENT_3D('',#10528,#8362,#8363);
#6613=AXIS2_PLACEMENT_3D('',#10529,#8364,#8365);
#6614=AXIS2_PLACEMENT_3D('',#10530,#8366,#8367);
#6615=AXIS2_PLACEMENT_3D('',#10531,#8368,#8369);
#6616=AXIS2_PLACEMENT_3D('',#10536,#8371,#8372);
#6617=AXIS2_PLACEMENT_3D('',#10537,#8373,#8374);
#6618=AXIS2_PLACEMENT_3D('',#10538,#8375,#8376);
#6619=AXIS2_PLACEMENT_3D('',#10591,#8378,#8379);
#6620=AXIS2_PLACEMENT_3D('',#10606,#8380,#8381);
#6621=AXIS2_PLACEMENT_3D('',#10608,#8383,#8384);
#6622=AXIS2_PLACEMENT_3D('',#10612,#8386,#8387);
#6623=AXIS2_PLACEMENT_3D('',#10613,#8388,#8389);
#6624=AXIS2_PLACEMENT_3D('',#10667,#8391,#8392);
#6625=AXIS2_PLACEMENT_3D('',#10693,#8393,#8394);
#6626=AXIS2_PLACEMENT_3D('',#10695,#8396,#8397);
#6627=AXIS2_PLACEMENT_3D('',#10697,#8398,#8399);
#6628=AXIS2_PLACEMENT_3D('',#10701,#8402,#8403);
#6629=AXIS2_PLACEMENT_3D('',#10702,#8404,#8405);
#6630=AXIS2_PLACEMENT_3D('',#10704,#8406,#8407);
#6631=AXIS2_PLACEMENT_3D('',#10708,#8410,#8411);
#6632=AXIS2_PLACEMENT_3D('',#10709,#8412,#8413);
#6633=AXIS2_PLACEMENT_3D('',#10710,#8414,#8415);
#6634=AXIS2_PLACEMENT_3D('',#10711,#8416,#8417);
#6635=AXIS2_PLACEMENT_3D('',#10712,#8418,#8419);
#6636=AXIS2_PLACEMENT_3D('',#10714,#8420,#8421);
#6637=AXIS2_PLACEMENT_3D('',#10715,#8422,#8423);
#6638=AXIS2_PLACEMENT_3D('',#10724,#8428,#8429);
#6639=AXIS2_PLACEMENT_3D('',#10730,#8433,#8434);
#6640=AXIS2_PLACEMENT_3D('',#10736,#8438,#8439);
#6641=AXIS2_PLACEMENT_3D('',#10742,#8443,#8444);
#6642=AXIS2_PLACEMENT_3D('',#10748,#8448,#8449);
#6643=AXIS2_PLACEMENT_3D('',#10751,#8452,#8453);
#6644=AXIS2_PLACEMENT_3D('',#10752,#8454,#8455);
#6645=AXIS2_PLACEMENT_3D('',#10754,#8456,#8457);
#6646=AXIS2_PLACEMENT_3D('',#10755,#8458,#8459);
#6647=AXIS2_PLACEMENT_3D('',#10757,#8460,#8461);
#6648=AXIS2_PLACEMENT_3D('',#10759,#8463,#8464);
#6649=AXIS2_PLACEMENT_3D('',#10761,#8466,#8467);
#6650=AXIS2_PLACEMENT_3D('',#10762,#8468,#8469);
#6651=AXIS2_PLACEMENT_3D('',#10763,#8470,#8471);
#6652=AXIS2_PLACEMENT_3D('',#10764,#8472,#8473);
#6653=AXIS2_PLACEMENT_3D('',#10765,#8474,#8475);
#6654=AXIS2_PLACEMENT_3D('',#10766,#8476,#8477);
#6655=AXIS2_PLACEMENT_3D('',#10767,#8478,#8479);
#6656=AXIS2_PLACEMENT_3D('',#10768,#8480,#8481);
#6657=AXIS2_PLACEMENT_3D('',#10769,#8482,#8483);
#6658=AXIS2_PLACEMENT_3D('',#10770,#8484,#8485);
#6659=AXIS2_PLACEMENT_3D('',#10771,#8486,#8487);
#6660=AXIS2_PLACEMENT_3D('',#10772,#8488,#8489);
#6661=AXIS2_PLACEMENT_3D('',#10773,#8490,#8491);
#6662=AXIS2_PLACEMENT_3D('',#10774,#8492,#8493);
#6663=AXIS2_PLACEMENT_3D('',#10775,#8494,#8495);
#6664=AXIS2_PLACEMENT_3D('',#10776,#8496,#8497);
#6665=AXIS2_PLACEMENT_3D('',#10777,#8498,#8499);
#6666=DIRECTION('axis',(0.,0.,1.));
#6667=DIRECTION('refdir',(1.,0.,0.));
#6668=DIRECTION('axis',(0.,0.,1.));
#6669=DIRECTION('refdir',(1.,0.,0.));
#6670=DIRECTION('axis',(0.,0.,1.));
#6671=DIRECTION('refdir',(1.,0.,0.));
#6672=DIRECTION('center_axis',(0.,0.,1.));
#6673=DIRECTION('ref_axis',(1.,0.,0.));
#6674=DIRECTION('center_axis',(0.,0.,1.));
#6675=DIRECTION('ref_axis',(1.,0.,0.));
#6676=DIRECTION('',(0.,0.,1.));
#6677=DIRECTION('center_axis',(0.,0.,-1.));
#6678=DIRECTION('ref_axis',(1.,0.,0.));
#6679=DIRECTION('center_axis',(0.,0.,1.));
#6680=DIRECTION('ref_axis',(1.,0.,0.));
#6681=DIRECTION('center_axis',(0.,0.,1.));
#6682=DIRECTION('ref_axis',(1.,0.,0.));
#6683=DIRECTION('center_axis',(0.,0.,1.));
#6684=DIRECTION('ref_axis',(1.,0.,0.));
#6685=DIRECTION('',(0.,0.,1.));
#6686=DIRECTION('center_axis',(0.,0.,-1.));
#6687=DIRECTION('ref_axis',(1.,0.,0.));
#6688=DIRECTION('center_axis',(0.,0.,1.));
#6689=DIRECTION('ref_axis',(1.,0.,0.));
#6690=DIRECTION('center_axis',(0.,0.,1.));
#6691=DIRECTION('ref_axis',(1.,0.,0.));
#6692=DIRECTION('center_axis',(0.,0.,1.));
#6693=DIRECTION('ref_axis',(1.,0.,0.));
#6694=DIRECTION('',(0.,0.,1.));
#6695=DIRECTION('center_axis',(0.,0.,-1.));
#6696=DIRECTION('ref_axis',(1.,0.,0.));
#6697=DIRECTION('center_axis',(0.,0.,1.));
#6698=DIRECTION('ref_axis',(1.,0.,0.));
#6699=DIRECTION('center_axis',(0.,0.,1.));
#6700=DIRECTION('ref_axis',(1.,0.,0.));
#6701=DIRECTION('center_axis',(0.,0.,1.));
#6702=DIRECTION('ref_axis',(1.,0.,0.));
#6703=DIRECTION('',(0.,0.,1.));
#6704=DIRECTION('center_axis',(0.,0.,-1.));
#6705=DIRECTION('ref_axis',(1.,0.,0.));
#6706=DIRECTION('center_axis',(0.,0.,1.));
#6707=DIRECTION('ref_axis',(1.,0.,0.));
#6708=DIRECTION('center_axis',(0.,0.,1.));
#6709=DIRECTION('ref_axis',(1.,0.,0.));
#6710=DIRECTION('center_axis',(0.,0.,1.));
#6711=DIRECTION('ref_axis',(1.,0.,0.));
#6712=DIRECTION('',(0.,0.,1.));
#6713=DIRECTION('center_axis',(0.,0.,-1.));
#6714=DIRECTION('ref_axis',(1.,0.,0.));
#6715=DIRECTION('center_axis',(0.,0.,1.));
#6716=DIRECTION('ref_axis',(1.,0.,0.));
#6717=DIRECTION('center_axis',(0.,0.,1.));
#6718=DIRECTION('ref_axis',(1.,0.,0.));
#6719=DIRECTION('center_axis',(0.,0.,1.));
#6720=DIRECTION('ref_axis',(1.,0.,0.));
#6721=DIRECTION('center_axis',(0.,0.,1.));
#6722=DIRECTION('ref_axis',(1.,0.,0.));
#6723=DIRECTION('',(0.,0.,1.));
#6724=DIRECTION('center_axis',(0.,0.,1.));
#6725=DIRECTION('ref_axis',(1.,0.,0.));
#6726=DIRECTION('center_axis',(0.,0.,1.));
#6727=DIRECTION('ref_axis',(1.,0.,0.));
#6728=DIRECTION('',(0.,0.,1.));
#6729=DIRECTION('center_axis',(0.,0.,-1.));
#6730=DIRECTION('ref_axis',(1.,0.,0.));
#6731=DIRECTION('center_axis',(0.,0.,1.));
#6732=DIRECTION('ref_axis',(1.,0.,0.));
#6733=DIRECTION('center_axis',(0.,0.,1.));
#6734=DIRECTION('ref_axis',(1.,0.,0.));
#6735=DIRECTION('center_axis',(0.,0.,1.));
#6736=DIRECTION('ref_axis',(1.,0.,0.));
#6737=DIRECTION('',(0.,0.,1.));
#6738=DIRECTION('center_axis',(0.,0.,-1.));
#6739=DIRECTION('ref_axis',(1.,0.,0.));
#6740=DIRECTION('center_axis',(0.,0.,1.));
#6741=DIRECTION('ref_axis',(1.,0.,0.));
#6742=DIRECTION('center_axis',(0.,0.,1.));
#6743=DIRECTION('ref_axis',(1.,0.,0.));
#6744=DIRECTION('center_axis',(0.,0.,1.));
#6745=DIRECTION('ref_axis',(1.,0.,0.));
#6746=DIRECTION('',(0.,0.,1.));
#6747=DIRECTION('center_axis',(0.,0.,-1.));
#6748=DIRECTION('ref_axis',(1.,0.,0.));
#6749=DIRECTION('center_axis',(0.,0.,1.));
#6750=DIRECTION('ref_axis',(1.,0.,0.));
#6751=DIRECTION('center_axis',(0.,0.,1.));
#6752=DIRECTION('ref_axis',(1.,0.,0.));
#6753=DIRECTION('center_axis',(0.,0.,1.));
#6754=DIRECTION('ref_axis',(1.,0.,0.));
#6755=DIRECTION('',(0.,0.,1.));
#6756=DIRECTION('center_axis',(0.,0.,-1.));
#6757=DIRECTION('ref_axis',(1.,0.,0.));
#6758=DIRECTION('center_axis',(0.,0.,1.));
#6759=DIRECTION('ref_axis',(1.,0.,0.));
#6760=DIRECTION('center_axis',(0.,0.,1.));
#6761=DIRECTION('ref_axis',(1.,0.,0.));
#6762=DIRECTION('center_axis',(0.,0.,1.));
#6763=DIRECTION('ref_axis',(1.,0.,0.));
#6764=DIRECTION('',(0.,0.,1.));
#6765=DIRECTION('center_axis',(0.,0.,-1.));
#6766=DIRECTION('ref_axis',(1.,0.,0.));
#6767=DIRECTION('center_axis',(0.,0.,1.));
#6768=DIRECTION('ref_axis',(1.,0.,0.));
#6769=DIRECTION('center_axis',(0.,0.,1.));
#6770=DIRECTION('ref_axis',(1.,0.,0.));
#6771=DIRECTION('center_axis',(0.,0.,1.));
#6772=DIRECTION('ref_axis',(1.,0.,0.));
#6773=DIRECTION('center_axis',(0.,0.,1.));
#6774=DIRECTION('ref_axis',(1.,0.,0.));
#6775=DIRECTION('',(0.,0.,1.));
#6776=DIRECTION('center_axis',(0.,0.,1.));
#6777=DIRECTION('ref_axis',(1.,0.,0.));
#6778=DIRECTION('center_axis',(0.,0.,1.));
#6779=DIRECTION('ref_axis',(1.,0.,0.));
#6780=DIRECTION('',(0.,0.,1.));
#6781=DIRECTION('center_axis',(0.,0.,-1.));
#6782=DIRECTION('ref_axis',(1.,0.,0.));
#6783=DIRECTION('center_axis',(0.,0.,1.));
#6784=DIRECTION('ref_axis',(1.,0.,0.));
#6785=DIRECTION('center_axis',(0.,0.,1.));
#6786=DIRECTION('ref_axis',(1.,0.,0.));
#6787=DIRECTION('center_axis',(0.,0.,1.));
#6788=DIRECTION('ref_axis',(1.,0.,0.));
#6789=DIRECTION('center_axis',(0.,0.,1.));
#6790=DIRECTION('ref_axis',(1.,0.,0.));
#6791=DIRECTION('',(0.,0.,1.));
#6792=DIRECTION('center_axis',(0.,0.,-1.));
#6793=DIRECTION('ref_axis',(1.,0.,0.));
#6794=DIRECTION('center_axis',(0.,0.,1.));
#6795=DIRECTION('ref_axis',(1.,0.,0.));
#6796=DIRECTION('center_axis',(0.,0.,1.));
#6797=DIRECTION('ref_axis',(1.,0.,0.));
#6798=DIRECTION('center_axis',(0.,0.,1.));
#6799=DIRECTION('ref_axis',(1.,0.,0.));
#6800=DIRECTION('center_axis',(0.,0.,1.));
#6801=DIRECTION('ref_axis',(1.,0.,0.));
#6802=DIRECTION('',(0.,0.,1.));
#6803=DIRECTION('center_axis',(0.,0.,-1.));
#6804=DIRECTION('ref_axis',(1.,0.,0.));
#6805=DIRECTION('center_axis',(0.,0.,1.));
#6806=DIRECTION('ref_axis',(1.,0.,0.));
#6807=DIRECTION('center_axis',(0.,0.,1.));
#6808=DIRECTION('ref_axis',(1.,0.,0.));
#6809=DIRECTION('center_axis',(0.,0.,1.));
#6810=DIRECTION('ref_axis',(1.,0.,0.));
#6811=DIRECTION('center_axis',(0.,0.,1.));
#6812=DIRECTION('ref_axis',(1.,0.,0.));
#6813=DIRECTION('',(0.,0.,1.));
#6814=DIRECTION('center_axis',(0.,0.,-1.));
#6815=DIRECTION('ref_axis',(1.,0.,0.));
#6816=DIRECTION('center_axis',(0.,0.,1.));
#6817=DIRECTION('ref_axis',(1.,0.,0.));
#6818=DIRECTION('center_axis',(0.,0.,1.));
#6819=DIRECTION('ref_axis',(1.,0.,0.));
#6820=DIRECTION('center_axis',(0.,0.,1.));
#6821=DIRECTION('ref_axis',(1.,0.,0.));
#6822=DIRECTION('center_axis',(0.,0.,1.));
#6823=DIRECTION('ref_axis',(1.,0.,0.));
#6824=DIRECTION('',(0.,0.,1.));
#6825=DIRECTION('center_axis',(0.,0.,1.));
#6826=DIRECTION('ref_axis',(1.,0.,0.));
#6827=DIRECTION('center_axis',(0.,0.,1.));
#6828=DIRECTION('ref_axis',(1.,0.,0.));
#6829=DIRECTION('',(0.,0.,1.));
#6830=DIRECTION('center_axis',(0.,0.,1.));
#6831=DIRECTION('ref_axis',(1.,0.,0.));
#6832=DIRECTION('center_axis',(0.,0.,1.));
#6833=DIRECTION('ref_axis',(1.,0.,0.));
#6834=DIRECTION('',(0.,0.,1.));
#6835=DIRECTION('center_axis',(0.,0.,1.));
#6836=DIRECTION('ref_axis',(1.,0.,0.));
#6837=DIRECTION('center_axis',(0.,0.,1.));
#6838=DIRECTION('ref_axis',(1.,0.,0.));
#6839=DIRECTION('',(0.,0.,1.));
#6840=DIRECTION('center_axis',(0.,0.,1.));
#6841=DIRECTION('ref_axis',(1.,0.,0.));
#6842=DIRECTION('center_axis',(0.,0.,-1.));
#6843=DIRECTION('ref_axis',(1.,0.,0.));
#6844=DIRECTION('center_axis',(0.,0.,1.));
#6845=DIRECTION('ref_axis',(1.,0.,0.));
#6846=DIRECTION('center_axis',(0.,0.,-1.));
#6847=DIRECTION('ref_axis',(1.,0.,0.));
#6848=DIRECTION('center_axis',(0.,0.,1.));
#6849=DIRECTION('ref_axis',(1.,0.,0.));
#6850=DIRECTION('center_axis',(0.,0.,-1.));
#6851=DIRECTION('ref_axis',(1.,0.,0.));
#6852=DIRECTION('center_axis',(0.,0.,1.));
#6853=DIRECTION('ref_axis',(1.,0.,0.));
#6854=DIRECTION('center_axis',(0.,0.,-1.));
#6855=DIRECTION('ref_axis',(1.,0.,0.));
#6856=DIRECTION('center_axis',(0.,0.,1.));
#6857=DIRECTION('ref_axis',(1.,0.,0.));
#6858=DIRECTION('center_axis',(0.,0.,1.));
#6859=DIRECTION('ref_axis',(1.,0.,0.));
#6860=DIRECTION('center_axis',(-1.,0.,0.));
#6861=DIRECTION('ref_axis',(0.,0.,1.));
#6862=DIRECTION('',(0.,1.,0.));
#6863=DIRECTION('',(0.,0.,-1.));
#6864=DIRECTION('',(0.,1.,0.));
#6865=DIRECTION('',(0.,0.,1.));
#6866=DIRECTION('center_axis',(0.,1.,0.));
#6867=DIRECTION('ref_axis',(0.,0.,1.));
#6868=DIRECTION('',(1.,0.,0.));
#6869=DIRECTION('',(-1.,0.,0.));
#6870=DIRECTION('',(0.,0.,-1.));
#6871=DIRECTION('center_axis',(1.,0.,0.));
#6872=DIRECTION('ref_axis',(0.,0.,-1.));
#6873=DIRECTION('',(0.,-1.,0.));
#6874=DIRECTION('',(0.,1.,0.));
#6875=DIRECTION('',(0.,0.,-1.));
#6876=DIRECTION('center_axis',(0.,-1.,0.));
#6877=DIRECTION('ref_axis',(1.,0.,0.));
#6878=DIRECTION('center_axis',(0.,1.,0.));
#6879=DIRECTION('ref_axis',(1.,0.,0.));
#6880=DIRECTION('',(0.,1.,0.));
#6881=DIRECTION('center_axis',(0.,-1.,0.));
#6882=DIRECTION('ref_axis',(1.,0.,0.));
#6883=DIRECTION('center_axis',(0.,1.,0.));
#6884=DIRECTION('ref_axis',(1.,0.,0.));
#6885=DIRECTION('',(0.,1.,0.));
#6886=DIRECTION('center_axis',(0.,0.,1.));
#6887=DIRECTION('ref_axis',(-1.,0.,0.));
#6888=DIRECTION('',(1.,0.,0.));
#6889=DIRECTION('center_axis',(0.,-1.,0.));
#6890=DIRECTION('ref_axis',(1.,0.,0.));
#6891=DIRECTION('',(-1.,0.,0.));
#6892=DIRECTION('center_axis',(0.,0.,1.));
#6893=DIRECTION('ref_axis',(1.,0.,0.));
#6894=DIRECTION('center_axis',(0.,0.,1.));
#6895=DIRECTION('ref_axis',(1.,0.,0.));
#6896=DIRECTION('',(0.,0.,1.));
#6897=DIRECTION('center_axis',(0.,0.,-1.));
#6898=DIRECTION('ref_axis',(1.,0.,0.));
#6899=DIRECTION('center_axis',(0.,0.,1.));
#6900=DIRECTION('ref_axis',(1.,0.,0.));
#6901=DIRECTION('center_axis',(0.,0.,1.));
#6902=DIRECTION('ref_axis',(1.,0.,0.));
#6903=DIRECTION('',(0.,0.,1.));
#6904=DIRECTION('center_axis',(0.,0.,-1.));
#6905=DIRECTION('ref_axis',(1.,0.,0.));
#6906=DIRECTION('center_axis',(0.,0.,1.));
#6907=DIRECTION('ref_axis',(1.,0.,0.));
#6908=DIRECTION('center_axis',(0.,0.,1.));
#6909=DIRECTION('ref_axis',(1.,0.,0.));
#6910=DIRECTION('',(0.,0.,1.));
#6911=DIRECTION('center_axis',(0.,0.,-1.));
#6912=DIRECTION('ref_axis',(1.,0.,0.));
#6913=DIRECTION('center_axis',(0.,0.,1.));
#6914=DIRECTION('ref_axis',(1.,0.,0.));
#6915=DIRECTION('center_axis',(0.,0.,1.));
#6916=DIRECTION('ref_axis',(1.,0.,0.));
#6917=DIRECTION('',(0.,0.,1.));
#6918=DIRECTION('center_axis',(0.,0.,-1.));
#6919=DIRECTION('ref_axis',(1.,0.,0.));
#6920=DIRECTION('center_axis',(0.,1.,0.));
#6921=DIRECTION('ref_axis',(-1.,0.,0.));
#6922=DIRECTION('',(-1.,0.,0.));
#6923=DIRECTION('',(0.,0.,1.));
#6924=DIRECTION('',(-1.,0.,0.));
#6925=DIRECTION('',(0.,0.,1.));
#6926=DIRECTION('center_axis',(1.,0.,0.));
#6927=DIRECTION('ref_axis',(0.,1.,0.));
#6928=DIRECTION('',(0.,1.,0.));
#6929=DIRECTION('',(0.,1.,0.));
#6930=DIRECTION('',(0.,0.,1.));
#6931=DIRECTION('center_axis',(0.,-1.,0.));
#6932=DIRECTION('ref_axis',(1.,0.,0.));
#6933=DIRECTION('',(1.,0.,0.));
#6934=DIRECTION('',(1.,0.,0.));
#6935=DIRECTION('',(0.,0.,1.));
#6936=DIRECTION('center_axis',(-1.,0.,0.));
#6937=DIRECTION('ref_axis',(0.,-1.,0.));
#6938=DIRECTION('',(0.,-1.,0.));
#6939=DIRECTION('',(0.,-1.,0.));
#6940=DIRECTION('center_axis',(0.,0.,1.));
#6941=DIRECTION('ref_axis',(1.,0.,0.));
#6942=DIRECTION('center_axis',(0.,0.,1.));
#6943=DIRECTION('ref_axis',(1.,0.,0.));
#6944=DIRECTION('',(0.,0.,1.));
#6945=DIRECTION('center_axis',(0.,0.,1.));
#6946=DIRECTION('ref_axis',(1.,0.,0.));
#6947=DIRECTION('center_axis',(0.,0.,1.));
#6948=DIRECTION('ref_axis',(1.,0.,0.));
#6949=DIRECTION('',(0.,0.,1.));
#6950=DIRECTION('center_axis',(0.,0.,1.));
#6951=DIRECTION('ref_axis',(1.,0.,0.));
#6952=DIRECTION('center_axis',(0.,0.,1.));
#6953=DIRECTION('ref_axis',(1.,0.,0.));
#6954=DIRECTION('',(0.,0.,1.));
#6955=DIRECTION('center_axis',(0.,0.,1.));
#6956=DIRECTION('ref_axis',(1.,0.,0.));
#6957=DIRECTION('center_axis',(0.,0.,1.));
#6958=DIRECTION('ref_axis',(1.,0.,0.));
#6959=DIRECTION('',(0.,0.,1.));
#6960=DIRECTION('center_axis',(0.,0.,1.));
#6961=DIRECTION('ref_axis',(1.,0.,0.));
#6962=DIRECTION('center_axis',(0.,0.,1.));
#6963=DIRECTION('ref_axis',(1.,0.,0.));
#6964=DIRECTION('axis',(0.,0.,1.));
#6965=DIRECTION('refdir',(1.,0.,0.));
#6966=DIRECTION('center_axis',(0.,1.,0.));
#6967=DIRECTION('ref_axis',(-1.,0.,0.));
#6968=DIRECTION('',(-1.,0.,0.));
#6969=DIRECTION('',(0.,0.,1.));
#6970=DIRECTION('',(-1.,0.,0.));
#6971=DIRECTION('',(0.,0.,1.));
#6972=DIRECTION('center_axis',(1.,0.,0.));
#6973=DIRECTION('ref_axis',(0.,1.,0.));
#6974=DIRECTION('',(0.,1.,0.));
#6975=DIRECTION('',(0.,1.,0.));
#6976=DIRECTION('',(0.,0.,1.));
#6977=DIRECTION('center_axis',(0.,-1.,0.));
#6978=DIRECTION('ref_axis',(1.,0.,0.));
#6979=DIRECTION('',(1.,0.,0.));
#6980=DIRECTION('',(1.,0.,0.));
#6981=DIRECTION('',(0.,0.,1.));
#6982=DIRECTION('center_axis',(-1.,0.,0.));
#6983=DIRECTION('ref_axis',(0.,-1.,0.));
#6984=DIRECTION('',(0.,-1.,0.));
#6985=DIRECTION('',(0.,-1.,0.));
#6986=DIRECTION('center_axis',(0.,0.,1.));
#6987=DIRECTION('ref_axis',(1.,0.,0.));
#6988=DIRECTION('center_axis',(0.,0.,1.));
#6989=DIRECTION('ref_axis',(1.,0.,0.));
#6990=DIRECTION('axis',(0.,0.,1.));
#6991=DIRECTION('refdir',(1.,0.,0.));
#6992=DIRECTION('center_axis',(0.,1.,0.));
#6993=DIRECTION('ref_axis',(-1.,0.,0.));
#6994=DIRECTION('',(-1.,0.,0.));
#6995=DIRECTION('',(0.,0.,1.));
#6996=DIRECTION('',(-1.,0.,0.));
#6997=DIRECTION('',(0.,0.,1.));
#6998=DIRECTION('center_axis',(1.,0.,0.));
#6999=DIRECTION('ref_axis',(0.,1.,0.));
#7000=DIRECTION('',(0.,1.,0.));
#7001=DIRECTION('',(0.,1.,0.));
#7002=DIRECTION('',(0.,0.,1.));
#7003=DIRECTION('center_axis',(0.,-1.,0.));
#7004=DIRECTION('ref_axis',(1.,0.,0.));
#7005=DIRECTION('',(1.,0.,0.));
#7006=DIRECTION('',(1.,0.,0.));
#7007=DIRECTION('',(0.,0.,1.));
#7008=DIRECTION('center_axis',(-1.,0.,0.));
#7009=DIRECTION('ref_axis',(0.,-1.,0.));
#7010=DIRECTION('',(0.,-1.,0.));
#7011=DIRECTION('',(0.,-1.,0.));
#7012=DIRECTION('center_axis',(0.,0.,1.));
#7013=DIRECTION('ref_axis',(1.,0.,0.));
#7014=DIRECTION('center_axis',(0.,0.,1.));
#7015=DIRECTION('ref_axis',(1.,0.,0.));
#7016=DIRECTION('axis',(0.,0.,1.));
#7017=DIRECTION('refdir',(1.,0.,0.));
#7018=DIRECTION('center_axis',(0.,0.,1.));
#7019=DIRECTION('ref_axis',(1.,0.,0.));
#7020=DIRECTION('',(0.,0.,1.));
#7021=DIRECTION('center_axis',(0.,0.,1.));
#7022=DIRECTION('ref_axis',(1.,0.,0.));
#7023=DIRECTION('',(0.,0.,-1.));
#7024=DIRECTION('center_axis',(0.,0.,-1.));
#7025=DIRECTION('ref_axis',(1.,0.,0.));
#7026=DIRECTION('center_axis',(0.,0.,1.));
#7027=DIRECTION('ref_axis',(1.,0.,0.));
#7028=DIRECTION('center_axis',(0.,0.,-1.));
#7029=DIRECTION('ref_axis',(1.,0.,0.));
#7030=DIRECTION('center_axis',(0.,0.,-1.));
#7031=DIRECTION('ref_axis',(1.,0.,0.));
#7032=DIRECTION('center_axis',(0.,0.,1.));
#7033=DIRECTION('ref_axis',(1.,0.,0.));
#7034=DIRECTION('center_axis',(0.,0.,1.));
#7035=DIRECTION('ref_axis',(1.,0.,0.));
#7036=DIRECTION('center_axis',(0.,0.,-1.));
#7037=DIRECTION('ref_axis',(1.,0.,0.));
#7038=DIRECTION('center_axis',(0.,0.,1.));
#7039=DIRECTION('ref_axis',(1.,0.,0.));
#7040=DIRECTION('center_axis',(0.,0.,1.));
#7041=DIRECTION('ref_axis',(1.,0.,0.));
#7042=DIRECTION('center_axis',(0.,0.,1.));
#7043=DIRECTION('ref_axis',(-1.83697019872103E-16,-1.,0.));
#7044=DIRECTION('',(0.,0.,-1.));
#7045=DIRECTION('center_axis',(0.,0.,-1.));
#7046=DIRECTION('ref_axis',(1.,0.,0.));
#7047=DIRECTION('',(0.,0.,1.));
#7048=DIRECTION('center_axis',(0.,0.,1.));
#7049=DIRECTION('ref_axis',(1.,0.,0.));
#7050=DIRECTION('center_axis',(0.,0.,-1.));
#7051=DIRECTION('ref_axis',(1.,0.,0.));
#7052=DIRECTION('center_axis',(0.,0.,1.));
#7053=DIRECTION('ref_axis',(1.,0.,0.));
#7054=DIRECTION('center_axis',(0.,0.,1.));
#7055=DIRECTION('ref_axis',(1.,0.,0.));
#7056=DIRECTION('center_axis',(0.,0.,1.));
#7057=DIRECTION('ref_axis',(-1.,1.22464679914735E-16,0.));
#7058=DIRECTION('',(0.,0.,-1.));
#7059=DIRECTION('center_axis',(0.,0.,-1.));
#7060=DIRECTION('ref_axis',(1.,0.,0.));
#7061=DIRECTION('',(0.,0.,1.));
#7062=DIRECTION('center_axis',(0.,0.,1.));
#7063=DIRECTION('ref_axis',(1.,0.,0.));
#7064=DIRECTION('center_axis',(0.,0.,-1.));
#7065=DIRECTION('ref_axis',(1.,0.,0.));
#7066=DIRECTION('center_axis',(0.,0.,1.));
#7067=DIRECTION('ref_axis',(1.,0.,0.));
#7068=DIRECTION('center_axis',(0.,0.,1.));
#7069=DIRECTION('ref_axis',(1.,0.,0.));
#7070=DIRECTION('center_axis',(0.,0.,1.));
#7071=DIRECTION('ref_axis',(6.12323399573677E-17,1.,0.));
#7072=DIRECTION('',(0.,0.,-1.));
#7073=DIRECTION('center_axis',(0.,0.,-1.));
#7074=DIRECTION('ref_axis',(1.,0.,0.));
#7075=DIRECTION('',(0.,0.,1.));
#7076=DIRECTION('center_axis',(0.,0.,1.));
#7077=DIRECTION('ref_axis',(1.,0.,0.));
#7078=DIRECTION('center_axis',(0.,0.,1.));
#7079=DIRECTION('ref_axis',(1.,0.,0.));
#7080=DIRECTION('center_axis',(0.,0.,1.));
#7081=DIRECTION('ref_axis',(1.,0.,0.));
#7082=DIRECTION('center_axis',(0.,0.,1.));
#7083=DIRECTION('ref_axis',(1.,0.,0.));
#7084=DIRECTION('center_axis',(0.,0.,1.));
#7085=DIRECTION('ref_axis',(1.,0.,0.));
#7086=DIRECTION('center_axis',(0.,0.,-1.));
#7087=DIRECTION('ref_axis',(1.,0.,0.));
#7088=DIRECTION('center_axis',(0.,0.,1.));
#7089=DIRECTION('ref_axis',(1.,0.,0.));
#7090=DIRECTION('center_axis',(0.,0.,1.));
#7091=DIRECTION('ref_axis',(1.,0.,0.));
#7092=DIRECTION('',(0.,0.,1.));
#7093=DIRECTION('center_axis',(0.,0.,1.));
#7094=DIRECTION('ref_axis',(1.,0.,0.));
#7095=DIRECTION('center_axis',(0.,0.,1.));
#7096=DIRECTION('ref_axis',(1.,0.,0.));
#7097=DIRECTION('',(0.,0.,1.));
#7098=DIRECTION('center_axis',(0.,0.,1.));
#7099=DIRECTION('ref_axis',(1.,0.,0.));
#7100=DIRECTION('center_axis',(0.,0.,1.));
#7101=DIRECTION('ref_axis',(1.,0.,0.));
#7102=DIRECTION('',(0.,0.,1.));
#7103=DIRECTION('center_axis',(0.,0.,1.));
#7104=DIRECTION('ref_axis',(1.,0.,0.));
#7105=DIRECTION('center_axis',(0.,0.,1.));
#7106=DIRECTION('ref_axis',(1.,0.,0.));
#7107=DIRECTION('',(0.,0.,1.));
#7108=DIRECTION('center_axis',(0.,0.,1.));
#7109=DIRECTION('ref_axis',(1.,0.,0.));
#7110=DIRECTION('center_axis',(0.,0.,1.));
#7111=DIRECTION('ref_axis',(1.,0.,0.));
#7112=DIRECTION('',(0.,0.,-1.));
#7113=DIRECTION('center_axis',(0.,0.,1.));
#7114=DIRECTION('ref_axis',(1.,0.,0.));
#7115=DIRECTION('center_axis',(0.,0.,1.));
#7116=DIRECTION('ref_axis',(1.,0.,0.));
#7117=DIRECTION('center_axis',(0.,0.,-1.));
#7118=DIRECTION('ref_axis',(1.,0.,0.));
#7119=DIRECTION('center_axis',(0.,0.,1.));
#7120=DIRECTION('ref_axis',(1.,0.,0.));
#7121=DIRECTION('',(0.,0.,-1.));
#7122=DIRECTION('center_axis',(0.,0.,1.));
#7123=DIRECTION('ref_axis',(1.,0.,0.));
#7124=DIRECTION('',(0.,0.,-1.));
#7125=DIRECTION('center_axis',(0.,0.,1.));
#7126=DIRECTION('ref_axis',(1.,0.,0.));
#7127=DIRECTION('center_axis',(0.,0.,1.));
#7128=DIRECTION('ref_axis',(1.,0.,0.));
#7129=DIRECTION('axis',(0.,0.,1.));
#7130=DIRECTION('refdir',(1.,0.,0.));
#7131=DIRECTION('center_axis',(0.,0.,1.));
#7132=DIRECTION('ref_axis',(1.,0.,0.));
#7133=DIRECTION('',(0.,0.,1.));
#7134=DIRECTION('center_axis',(0.,0.,1.));
#7135=DIRECTION('ref_axis',(1.,0.,0.));
#7136=DIRECTION('',(0.,0.,-1.));
#7137=DIRECTION('center_axis',(0.,0.,-1.));
#7138=DIRECTION('ref_axis',(1.,0.,0.));
#7139=DIRECTION('center_axis',(0.,0.,1.));
#7140=DIRECTION('ref_axis',(1.,0.,0.));
#7141=DIRECTION('center_axis',(0.,0.,-1.));
#7142=DIRECTION('ref_axis',(1.,0.,0.));
#7143=DIRECTION('center_axis',(0.,0.,-1.));
#7144=DIRECTION('ref_axis',(1.,0.,0.));
#7145=DIRECTION('center_axis',(0.,0.,1.));
#7146=DIRECTION('ref_axis',(1.,0.,0.));
#7147=DIRECTION('center_axis',(0.,0.,1.));
#7148=DIRECTION('ref_axis',(1.,0.,0.));
#7149=DIRECTION('center_axis',(0.,0.,-1.));
#7150=DIRECTION('ref_axis',(1.,0.,0.));
#7151=DIRECTION('center_axis',(0.,0.,1.));
#7152=DIRECTION('ref_axis',(1.,0.,0.));
#7153=DIRECTION('center_axis',(0.,0.,1.));
#7154=DIRECTION('ref_axis',(1.,0.,0.));
#7155=DIRECTION('center_axis',(0.,0.,1.));
#7156=DIRECTION('ref_axis',(-1.83697019872103E-16,-1.,0.));
#7157=DIRECTION('',(0.,0.,-1.));
#7158=DIRECTION('center_axis',(0.,0.,-1.));
#7159=DIRECTION('ref_axis',(1.,0.,0.));
#7160=DIRECTION('',(0.,0.,1.));
#7161=DIRECTION('center_axis',(0.,0.,1.));
#7162=DIRECTION('ref_axis',(1.,0.,0.));
#7163=DIRECTION('center_axis',(0.,0.,-1.));
#7164=DIRECTION('ref_axis',(1.,0.,0.));
#7165=DIRECTION('center_axis',(0.,0.,1.));
#7166=DIRECTION('ref_axis',(1.,0.,0.));
#7167=DIRECTION('center_axis',(0.,0.,1.));
#7168=DIRECTION('ref_axis',(1.,0.,0.));
#7169=DIRECTION('center_axis',(0.,0.,1.));
#7170=DIRECTION('ref_axis',(-1.,1.22464679914735E-16,0.));
#7171=DIRECTION('',(0.,0.,-1.));
#7172=DIRECTION('center_axis',(0.,0.,-1.));
#7173=DIRECTION('ref_axis',(1.,0.,0.));
#7174=DIRECTION('',(0.,0.,1.));
#7175=DIRECTION('center_axis',(0.,0.,1.));
#7176=DIRECTION('ref_axis',(1.,0.,0.));
#7177=DIRECTION('center_axis',(0.,0.,-1.));
#7178=DIRECTION('ref_axis',(1.,0.,0.));
#7179=DIRECTION('center_axis',(0.,0.,1.));
#7180=DIRECTION('ref_axis',(1.,0.,0.));
#7181=DIRECTION('center_axis',(0.,0.,1.));
#7182=DIRECTION('ref_axis',(1.,0.,0.));
#7183=DIRECTION('center_axis',(0.,0.,1.));
#7184=DIRECTION('ref_axis',(-6.04901474817726E-16,1.,0.));
#7185=DIRECTION('',(0.,0.,-1.));
#7186=DIRECTION('center_axis',(0.,0.,-1.));
#7187=DIRECTION('ref_axis',(1.,0.,0.));
#7188=DIRECTION('',(0.,0.,1.));
#7189=DIRECTION('center_axis',(0.,0.,1.));
#7190=DIRECTION('ref_axis',(1.,0.,0.));
#7191=DIRECTION('center_axis',(0.,0.,1.));
#7192=DIRECTION('ref_axis',(1.,0.,0.));
#7193=DIRECTION('center_axis',(0.,0.,1.));
#7194=DIRECTION('ref_axis',(1.,0.,0.));
#7195=DIRECTION('center_axis',(0.,0.,1.));
#7196=DIRECTION('ref_axis',(1.,0.,0.));
#7197=DIRECTION('center_axis',(0.,0.,1.));
#7198=DIRECTION('ref_axis',(1.,0.,0.));
#7199=DIRECTION('center_axis',(0.,0.,-1.));
#7200=DIRECTION('ref_axis',(1.,0.,0.));
#7201=DIRECTION('center_axis',(0.,0.,1.));
#7202=DIRECTION('ref_axis',(1.,0.,0.));
#7203=DIRECTION('center_axis',(0.,0.,1.));
#7204=DIRECTION('ref_axis',(1.,0.,0.));
#7205=DIRECTION('',(0.,0.,1.));
#7206=DIRECTION('center_axis',(0.,0.,1.));
#7207=DIRECTION('ref_axis',(1.,0.,0.));
#7208=DIRECTION('center_axis',(0.,0.,1.));
#7209=DIRECTION('ref_axis',(1.,0.,0.));
#7210=DIRECTION('',(0.,0.,1.));
#7211=DIRECTION('center_axis',(0.,0.,1.));
#7212=DIRECTION('ref_axis',(1.,0.,0.));
#7213=DIRECTION('center_axis',(0.,0.,1.));
#7214=DIRECTION('ref_axis',(1.,0.,0.));
#7215=DIRECTION('',(0.,0.,1.));
#7216=DIRECTION('center_axis',(0.,0.,1.));
#7217=DIRECTION('ref_axis',(1.,0.,0.));
#7218=DIRECTION('center_axis',(0.,0.,1.));
#7219=DIRECTION('ref_axis',(1.,0.,0.));
#7220=DIRECTION('',(0.,0.,1.));
#7221=DIRECTION('center_axis',(0.,0.,1.));
#7222=DIRECTION('ref_axis',(1.,0.,0.));
#7223=DIRECTION('center_axis',(0.,0.,1.));
#7224=DIRECTION('ref_axis',(1.,0.,0.));
#7225=DIRECTION('',(0.,0.,-1.));
#7226=DIRECTION('center_axis',(0.,0.,1.));
#7227=DIRECTION('ref_axis',(1.,0.,0.));
#7228=DIRECTION('center_axis',(0.,0.,1.));
#7229=DIRECTION('ref_axis',(1.,0.,0.));
#7230=DIRECTION('center_axis',(0.,0.,-1.));
#7231=DIRECTION('ref_axis',(1.,0.,0.));
#7232=DIRECTION('center_axis',(0.,0.,1.));
#7233=DIRECTION('ref_axis',(1.,0.,0.));
#7234=DIRECTION('',(0.,0.,-1.));
#7235=DIRECTION('center_axis',(0.,0.,1.));
#7236=DIRECTION('ref_axis',(1.,0.,0.));
#7237=DIRECTION('',(0.,0.,-1.));
#7238=DIRECTION('center_axis',(0.,0.,1.));
#7239=DIRECTION('ref_axis',(1.,0.,0.));
#7240=DIRECTION('center_axis',(0.,0.,1.));
#7241=DIRECTION('ref_axis',(1.,0.,0.));
#7242=DIRECTION('axis',(0.,0.,1.));
#7243=DIRECTION('refdir',(1.,0.,0.));
#7244=DIRECTION('center_axis',(0.,1.,0.));
#7245=DIRECTION('ref_axis',(0.,0.,1.));
#7246=DIRECTION('center_axis',(0.,-1.,0.));
#7247=DIRECTION('ref_axis',(1.,0.,0.));
#7248=DIRECTION('center_axis',(0.,-1.,0.));
#7249=DIRECTION('ref_axis',(1.,0.,0.));
#7250=DIRECTION('center_axis',(0.,-1.,0.));
#7251=DIRECTION('ref_axis',(1.,0.,0.));
#7252=DIRECTION('',(0.707106781186548,0.707106781186547,8.65956056235493E-17));
#7253=DIRECTION('center_axis',(0.,-1.,0.));
#7254=DIRECTION('ref_axis',(1.,0.,0.));
#7255=DIRECTION('center_axis',(0.,-1.,0.));
#7256=DIRECTION('ref_axis',(1.,0.,0.));
#7257=DIRECTION('',(0.,1.,0.));
#7258=DIRECTION('center_axis',(0.,1.,0.));
#7259=DIRECTION('ref_axis',(1.,0.,0.));
#7260=DIRECTION('center_axis',(0.,-1.,0.));
#7261=DIRECTION('ref_axis',(1.,0.,0.));
#7262=DIRECTION('',(-0.707106781186547,0.707106781186548,-8.65956056235493E-17));
#7263=DIRECTION('center_axis',(0.,-1.,0.));
#7264=DIRECTION('ref_axis',(0.,0.,-1.));
#7265=DIRECTION('center_axis',(0.,-1.,0.));
#7266=DIRECTION('ref_axis',(1.,0.,0.));
#7267=DIRECTION('center_axis',(0.,1.,0.));
#7268=DIRECTION('ref_axis',(1.,0.,0.));
#7269=DIRECTION('center_axis',(0.,1.,0.));
#7270=DIRECTION('ref_axis',(1.,0.,0.));
#7271=DIRECTION('',(-0.447213595499958,0.894427190999916,-5.47678698264203E-17));
#7272=DIRECTION('center_axis',(0.,-1.,0.));
#7273=DIRECTION('ref_axis',(1.,0.,0.));
#7274=DIRECTION('center_axis',(0.,1.,0.));
#7275=DIRECTION('ref_axis',(1.,0.,0.));
#7276=DIRECTION('',(0.,1.,0.));
#7277=DIRECTION('center_axis',(0.,1.,0.));
#7278=DIRECTION('ref_axis',(1.,0.,0.));
#7279=DIRECTION('center_axis',(0.,-1.,0.));
#7280=DIRECTION('ref_axis',(1.,0.,0.));
#7281=DIRECTION('',(-0.707106781186547,0.707106781186548,-8.65956056235493E-17));
#7282=DIRECTION('center_axis',(0.,-1.,0.));
#7283=DIRECTION('ref_axis',(0.,0.,-1.));
#7284=DIRECTION('center_axis',(0.866025403784439,0.,-0.5));
#7285=DIRECTION('ref_axis',(0.5,0.,0.866025403784439));
#7286=DIRECTION('',(-0.5,0.,-0.866025403784439));
#7287=DIRECTION('',(0.,-1.,0.));
#7288=DIRECTION('',(0.5,0.,0.866025403784439));
#7289=DIRECTION('',(0.,-1.,0.));
#7290=DIRECTION('center_axis',(1.20185167898973E-16,0.,-1.));
#7291=DIRECTION('ref_axis',(1.,0.,1.20185167898973E-16));
#7292=DIRECTION('',(-1.,0.,-1.20185167898973E-16));
#7293=DIRECTION('',(0.,-1.,0.));
#7294=DIRECTION('',(1.,0.,1.20185167898973E-16));
#7295=DIRECTION('center_axis',(-0.866025403784439,0.,-0.5));
#7296=DIRECTION('ref_axis',(0.5,0.,-0.866025403784439));
#7297=DIRECTION('',(-0.5,0.,0.866025403784439));
#7298=DIRECTION('',(0.,-1.,0.));
#7299=DIRECTION('',(0.5,0.,-0.866025403784439));
#7300=DIRECTION('center_axis',(-0.866025403784439,0.,0.5));
#7301=DIRECTION('ref_axis',(-0.5,0.,-0.866025403784439));
#7302=DIRECTION('',(0.5,0.,0.866025403784439));
#7303=DIRECTION('',(0.,-1.,0.));
#7304=DIRECTION('',(-0.5,0.,-0.866025403784439));
#7305=DIRECTION('center_axis',(-2.40370335797945E-16,0.,1.));
#7306=DIRECTION('ref_axis',(-1.,0.,-2.40370335797945E-16));
#7307=DIRECTION('',(1.,0.,2.40370335797945E-16));
#7308=DIRECTION('',(0.,-1.,0.));
#7309=DIRECTION('',(-1.,0.,-2.40370335797945E-16));
#7310=DIRECTION('center_axis',(0.866025403784439,0.,0.5));
#7311=DIRECTION('ref_axis',(-0.5,0.,0.866025403784439));
#7312=DIRECTION('',(0.5,0.,-0.866025403784439));
#7313=DIRECTION('',(-0.5,0.,0.866025403784439));
#7314=DIRECTION('center_axis',(0.,1.,0.));
#7315=DIRECTION('ref_axis',(1.,0.,0.));
#7316=DIRECTION('center_axis',(0.,-1.,0.));
#7317=DIRECTION('ref_axis',(0.,0.,-1.));
#7318=DIRECTION('axis',(0.,0.,1.));
#7319=DIRECTION('refdir',(1.,0.,0.));
#7320=DIRECTION('axis',(0.,0.,1.));
#7321=DIRECTION('refdir',(1.,0.,0.));
#7322=DIRECTION('center_axis',(0.,-1.,0.));
#7323=DIRECTION('ref_axis',(0.,0.,-1.));
#7324=DIRECTION('center_axis',(0.,-1.,0.));
#7325=DIRECTION('ref_axis',(1.,0.,0.));
#7326=DIRECTION('center_axis',(0.,-1.,0.));
#7327=DIRECTION('ref_axis',(1.,0.,0.));
#7328=DIRECTION('center_axis',(1.,0.,1.22464679914735E-16));
#7329=DIRECTION('ref_axis',(-1.22464679914735E-16,0.,1.));
#7330=DIRECTION('center_axis',(0.,1.,0.));
#7331=DIRECTION('ref_axis',(1.,0.,0.));
#7332=DIRECTION('center_axis',(0.,1.,0.));
#7333=DIRECTION('ref_axis',(1.,0.,0.));
#7334=DIRECTION('center_axis',(0.,-1.,0.));
#7335=DIRECTION('ref_axis',(1.,0.,0.));
#7336=DIRECTION('',(0.,1.,0.));
#7337=DIRECTION('center_axis',(0.,-1.,0.));
#7338=DIRECTION('ref_axis',(1.,0.,0.));
#7339=DIRECTION('center_axis',(0.,-1.,0.));
#7340=DIRECTION('ref_axis',(1.,0.,0.));
#7341=DIRECTION('center_axis',(0.,-1.,0.));
#7342=DIRECTION('ref_axis',(1.,0.,0.));
#7343=DIRECTION('',(0.,1.,0.));
#7344=DIRECTION('center_axis',(0.,-1.,0.));
#7345=DIRECTION('ref_axis',(1.,0.,0.));
#7346=DIRECTION('center_axis',(0.,1.,0.));
#7347=DIRECTION('ref_axis',(1.,0.,0.));
#7348=DIRECTION('',(-0.707106781186547,0.707106781186548,-8.65956056235493E-17));
#7349=DIRECTION('center_axis',(0.,-1.,0.));
#7350=DIRECTION('ref_axis',(1.,0.,0.));
#7351=DIRECTION('center_axis',(0.,1.,0.));
#7352=DIRECTION('ref_axis',(0.,0.,1.));
#7353=DIRECTION('center_axis',(0.,-1.,0.));
#7354=DIRECTION('ref_axis',(1.,0.,0.));
#7355=DIRECTION('center_axis',(0.,-1.,0.));
#7356=DIRECTION('ref_axis',(1.,0.,0.));
#7357=DIRECTION('',(0.,1.,0.));
#7358=DIRECTION('center_axis',(0.,-1.,0.));
#7359=DIRECTION('ref_axis',(0.,0.,-1.));
#7360=DIRECTION('center_axis',(0.,-1.,0.));
#7361=DIRECTION('ref_axis',(1.,0.,0.));
#7362=DIRECTION('center_axis',(0.,-1.,0.));
#7363=DIRECTION('ref_axis',(1.,0.,0.));
#7364=DIRECTION('',(0.707106781186547,0.707106781186548,8.65956056235493E-17));
#7365=DIRECTION('axis',(0.,0.,1.));
#7366=DIRECTION('refdir',(1.,0.,0.));
#7367=DIRECTION('center_axis',(0.,-1.,0.));
#7368=DIRECTION('ref_axis',(0.,0.,-1.));
#7369=DIRECTION('center_axis',(0.,-1.,0.));
#7370=DIRECTION('ref_axis',(1.,0.,0.));
#7371=DIRECTION('center_axis',(0.,-1.,0.));
#7372=DIRECTION('ref_axis',(1.,0.,0.));
#7373=DIRECTION('center_axis',(1.,0.,1.22464679914735E-16));
#7374=DIRECTION('ref_axis',(-1.22464679914735E-16,0.,1.));
#7375=DIRECTION('center_axis',(0.,1.,0.));
#7376=DIRECTION('ref_axis',(1.,0.,0.));
#7377=DIRECTION('center_axis',(0.,1.,0.));
#7378=DIRECTION('ref_axis',(1.,0.,0.));
#7379=DIRECTION('center_axis',(0.,-1.,0.));
#7380=DIRECTION('ref_axis',(1.,0.,0.));
#7381=DIRECTION('center_axis',(0.,-1.,0.));
#7382=DIRECTION('ref_axis',(1.,0.,0.));
#7383=DIRECTION('',(0.,1.,0.));
#7384=DIRECTION('center_axis',(0.,1.,0.));
#7385=DIRECTION('ref_axis',(0.,0.,1.));
#7386=DIRECTION('center_axis',(0.,-1.,0.));
#7387=DIRECTION('ref_axis',(1.,0.,0.));
#7388=DIRECTION('center_axis',(0.,-1.,0.));
#7389=DIRECTION('ref_axis',(1.,0.,0.));
#7390=DIRECTION('center_axis',(0.,-1.,0.));
#7391=DIRECTION('ref_axis',(1.,0.,0.));
#7392=DIRECTION('center_axis',(0.,-1.,0.));
#7393=DIRECTION('ref_axis',(1.,0.,0.));
#7394=DIRECTION('',(0.707106781186548,0.707106781186547,8.65956056235494E-17));
#7395=DIRECTION('center_axis',(0.,-1.,0.));
#7396=DIRECTION('ref_axis',(1.,0.,0.));
#7397=DIRECTION('center_axis',(0.,-1.,0.));
#7398=DIRECTION('ref_axis',(1.,0.,0.));
#7399=DIRECTION('',(0.,1.,0.));
#7400=DIRECTION('center_axis',(0.,1.,0.));
#7401=DIRECTION('ref_axis',(1.,0.,0.));
#7402=DIRECTION('center_axis',(0.,-1.,0.));
#7403=DIRECTION('ref_axis',(1.,0.,0.));
#7404=DIRECTION('',(-0.707106781186548,0.707106781186547,-8.65956056235494E-17));
#7405=DIRECTION('center_axis',(0.,-1.,0.));
#7406=DIRECTION('ref_axis',(0.,0.,-1.));
#7407=DIRECTION('center_axis',(0.,-1.,0.));
#7408=DIRECTION('ref_axis',(1.,0.,0.));
#7409=DIRECTION('',(0.,1.,0.));
#7410=DIRECTION('axis',(0.,0.,1.));
#7411=DIRECTION('refdir',(1.,0.,0.));
#7412=DIRECTION('center_axis',(0.,0.,1.));
#7413=DIRECTION('ref_axis',(1.,0.,0.));
#7414=DIRECTION('center_axis',(1.22464679914735E-16,-1.,0.));
#7415=DIRECTION('ref_axis',(-1.,-1.22464679914735E-16,0.));
#7416=DIRECTION('center_axis',(0.707106781186548,0.,0.707106781186548));
#7417=DIRECTION('ref_axis',(0.707106781186548,0.,-0.707106781186548));
#7418=DIRECTION('center_axis',(8.65956056235494E-17,-1.,-8.65956056235493E-17));
#7419=DIRECTION('ref_axis',(-0.707106781186547,-1.22464679914735E-16,0.707106781186547));
#7420=DIRECTION('center_axis',(1.,0.,0.));
#7421=DIRECTION('ref_axis',(6.12323399573676E-17,0.,-1.));
#7422=DIRECTION('center_axis',(7.49879891330929E-33,-1.,-1.22464679914735E-16));
#7423=DIRECTION('ref_axis',(-6.12323399573676E-17,-1.22464679914735E-16,
1.));
#7424=DIRECTION('center_axis',(0.707106781186548,0.,-0.707106781186548));
#7425=DIRECTION('ref_axis',(-0.707106781186548,0.,-0.707106781186548));
#7426=DIRECTION('center_axis',(-8.65956056235493E-17,-1.,-8.65956056235494E-17));
#7427=DIRECTION('ref_axis',(0.707106781186547,-1.22464679914735E-16,0.707106781186547));
#7428=DIRECTION('center_axis',(0.,0.,-1.));
#7429=DIRECTION('ref_axis',(-1.,0.,-1.22464679914735E-16));
#7430=DIRECTION('center_axis',(-1.22464679914735E-16,-1.,-1.49975978266186E-32));
#7431=DIRECTION('ref_axis',(1.,-1.22464679914735E-16,1.22464679914735E-16));
#7432=DIRECTION('center_axis',(-0.707106781186547,0.,-0.707106781186548));
#7433=DIRECTION('ref_axis',(-0.707106781186548,0.,0.707106781186547));
#7434=DIRECTION('center_axis',(-8.65956056235493E-17,-1.,8.65956056235493E-17));
#7435=DIRECTION('ref_axis',(0.707106781186548,-1.22464679914735E-16,-0.707106781186547));
#7436=DIRECTION('center_axis',(-1.,0.,0.));
#7437=DIRECTION('ref_axis',(-1.83697019872103E-16,0.,1.));
#7438=DIRECTION('center_axis',(-2.24963967399279E-32,-1.,1.22464679914735E-16));
#7439=DIRECTION('ref_axis',(1.83697019872103E-16,-1.22464679914735E-16,
-1.));
#7440=DIRECTION('center_axis',(-0.707106781186548,0.,0.707106781186548));
#7441=DIRECTION('ref_axis',(0.707106781186547,0.,0.707106781186548));
#7442=DIRECTION('center_axis',(8.65956056235493E-17,-1.,8.65956056235493E-17));
#7443=DIRECTION('ref_axis',(-0.707106781186547,-1.22464679914735E-16,-0.707106781186548));
#7444=DIRECTION('axis',(0.,0.,1.));
#7445=DIRECTION('refdir',(1.,0.,0.));
#7446=DIRECTION('center_axis',(0.,0.,1.));
#7447=DIRECTION('ref_axis',(1.,0.,0.));
#7448=DIRECTION('center_axis',(0.,-1.,0.));
#7449=DIRECTION('ref_axis',(0.,0.,-1.));
#7450=DIRECTION('center_axis',(0.,-1.,0.));
#7451=DIRECTION('ref_axis',(0.,0.,-1.));
#7452=DIRECTION('center_axis',(0.,1.,0.));
#7453=DIRECTION('ref_axis',(1.,0.,0.));
#7454=DIRECTION('center_axis',(0.,1.,0.));
#7455=DIRECTION('ref_axis',(1.,0.,0.));
#7456=DIRECTION('center_axis',(0.,1.,0.));
#7457=DIRECTION('ref_axis',(1.,0.,0.));
#7458=DIRECTION('center_axis',(0.,1.,0.));
#7459=DIRECTION('ref_axis',(1.,0.,0.));
#7460=DIRECTION('',(0.,-1.,0.));
#7461=DIRECTION('center_axis',(0.,-1.,0.));
#7462=DIRECTION('ref_axis',(1.,0.,0.));
#7463=DIRECTION('center_axis',(0.,1.,0.));
#7464=DIRECTION('ref_axis',(1.,0.,0.));
#7465=DIRECTION('center_axis',(0.,1.,0.));
#7466=DIRECTION('ref_axis',(1.,0.,0.));
#7467=DIRECTION('center_axis',(0.,1.,0.));
#7468=DIRECTION('ref_axis',(1.,0.,0.));
#7469=DIRECTION('center_axis',(0.,1.,0.));
#7470=DIRECTION('ref_axis',(1.,0.,0.));
#7471=DIRECTION('center_axis',(0.,1.,0.));
#7472=DIRECTION('ref_axis',(1.,0.,0.));
#7473=DIRECTION('center_axis',(0.,1.,0.));
#7474=DIRECTION('ref_axis',(1.,0.,0.));
#7475=DIRECTION('center_axis',(0.,-1.,0.));
#7476=DIRECTION('ref_axis',(1.,0.,0.));
#7477=DIRECTION('center_axis',(0.,-1.,0.));
#7478=DIRECTION('ref_axis',(0.,0.,-1.));
#7479=DIRECTION('center_axis',(6.12323399573677E-17,0.,1.));
#7480=DIRECTION('ref_axis',(1.,0.,0.));
#7481=DIRECTION('center_axis',(0.,-1.,0.));
#7482=DIRECTION('ref_axis',(0.,0.,-1.));
#7483=DIRECTION('center_axis',(0.,1.,0.));
#7484=DIRECTION('ref_axis',(1.,0.,0.));
#7485=DIRECTION('center_axis',(0.,-1.,0.));
#7486=DIRECTION('ref_axis',(1.,0.,0.));
#7487=DIRECTION('center_axis',(0.,-1.,0.));
#7488=DIRECTION('ref_axis',(0.,0.,-1.));
#7489=DIRECTION('center_axis',(0.,0.,1.));
#7490=DIRECTION('ref_axis',(1.,0.,0.));
#7491=DIRECTION('center_axis',(0.,-1.,0.));
#7492=DIRECTION('ref_axis',(0.,0.,-1.));
#7493=DIRECTION('center_axis',(0.,1.,0.));
#7494=DIRECTION('ref_axis',(1.,0.,0.));
#7495=DIRECTION('center_axis',(0.,-1.,0.));
#7496=DIRECTION('ref_axis',(1.,0.,0.));
#7497=DIRECTION('center_axis',(0.,-1.,0.));
#7498=DIRECTION('ref_axis',(0.,0.,-1.));
#7499=DIRECTION('center_axis',(0.,0.,1.));
#7500=DIRECTION('ref_axis',(1.,0.,0.));
#7501=DIRECTION('center_axis',(0.,-1.,0.));
#7502=DIRECTION('ref_axis',(0.,0.,-1.));
#7503=DIRECTION('center_axis',(0.,1.,0.));
#7504=DIRECTION('ref_axis',(1.,0.,0.));
#7505=DIRECTION('center_axis',(0.,-1.,0.));
#7506=DIRECTION('ref_axis',(1.,0.,0.));
#7507=DIRECTION('center_axis',(0.,-1.,0.));
#7508=DIRECTION('ref_axis',(0.,0.,-1.));
#7509=DIRECTION('center_axis',(0.,0.,1.));
#7510=DIRECTION('ref_axis',(1.,0.,0.));
#7511=DIRECTION('center_axis',(0.,-1.,0.));
#7512=DIRECTION('ref_axis',(0.,0.,-1.));
#7513=DIRECTION('center_axis',(0.,1.,0.));
#7514=DIRECTION('ref_axis',(1.,0.,0.));
#7515=DIRECTION('center_axis',(0.,-1.,0.));
#7516=DIRECTION('ref_axis',(1.,0.,0.));
#7517=DIRECTION('center_axis',(0.,-1.,0.));
#7518=DIRECTION('ref_axis',(0.,0.,-1.));
#7519=DIRECTION('center_axis',(6.12323399573676E-17,0.,1.));
#7520=DIRECTION('ref_axis',(1.,0.,0.));
#7521=DIRECTION('center_axis',(0.,-1.,0.));
#7522=DIRECTION('ref_axis',(0.,0.,-1.));
#7523=DIRECTION('center_axis',(0.,1.,0.));
#7524=DIRECTION('ref_axis',(1.,0.,0.));
#7525=DIRECTION('center_axis',(0.,-1.,0.));
#7526=DIRECTION('ref_axis',(1.,0.,0.));
#7527=DIRECTION('center_axis',(0.,-1.,0.));
#7528=DIRECTION('ref_axis',(0.,0.,-1.));
#7529=DIRECTION('center_axis',(0.,0.,1.));
#7530=DIRECTION('ref_axis',(1.,0.,0.));
#7531=DIRECTION('center_axis',(0.,-1.,0.));
#7532=DIRECTION('ref_axis',(0.,0.,-1.));
#7533=DIRECTION('center_axis',(0.,1.,0.));
#7534=DIRECTION('ref_axis',(1.,0.,0.));
#7535=DIRECTION('center_axis',(0.,1.,0.));
#7536=DIRECTION('ref_axis',(1.,0.,0.));
#7537=DIRECTION('',(0.,1.,0.));
#7538=DIRECTION('center_axis',(0.,-1.,0.));
#7539=DIRECTION('ref_axis',(1.,0.,0.));
#7540=DIRECTION('center_axis',(0.,-1.,0.));
#7541=DIRECTION('ref_axis',(1.,0.,0.));
#7542=DIRECTION('center_axis',(0.,1.,0.));
#7543=DIRECTION('ref_axis',(1.,0.,0.));
#7544=DIRECTION('center_axis',(0.,-1.,0.));
#7545=DIRECTION('ref_axis',(0.,0.,-1.));
#7546=DIRECTION('center_axis',(0.,0.,1.));
#7547=DIRECTION('ref_axis',(1.,0.,0.));
#7548=DIRECTION('center_axis',(0.,-1.,0.));
#7549=DIRECTION('ref_axis',(0.,0.,-1.));
#7550=DIRECTION('center_axis',(0.,-1.,0.));
#7551=DIRECTION('ref_axis',(-1.,0.,0.));
#7552=DIRECTION('center_axis',(0.,1.,0.));
#7553=DIRECTION('ref_axis',(1.,0.,0.));
#7554=DIRECTION('axis',(0.,0.,1.));
#7555=DIRECTION('refdir',(1.,0.,0.));
#7556=DIRECTION('center_axis',(0.,1.,0.));
#7557=DIRECTION('ref_axis',(0.,0.,1.));
#7558=DIRECTION('center_axis',(0.,-1.,0.));
#7559=DIRECTION('ref_axis',(1.,0.,0.));
#7560=DIRECTION('center_axis',(0.,-1.,0.));
#7561=DIRECTION('ref_axis',(1.,0.,0.));
#7562=DIRECTION('center_axis',(0.,-1.,0.));
#7563=DIRECTION('ref_axis',(1.,0.,0.));
#7564=DIRECTION('center_axis',(0.,-1.,0.));
#7565=DIRECTION('ref_axis',(1.,0.,0.));
#7566=DIRECTION('',(0.,1.,0.));
#7567=DIRECTION('center_axis',(0.,-1.,0.));
#7568=DIRECTION('ref_axis',(0.,0.,-1.));
#7569=DIRECTION('center_axis',(0.,-1.,0.));
#7570=DIRECTION('ref_axis',(1.,0.,0.));
#7571=DIRECTION('center_axis',(0.,-1.,0.));
#7572=DIRECTION('ref_axis',(1.,0.,0.));
#7573=DIRECTION('',(0.,1.,0.));
#7574=DIRECTION('center_axis',(0.,1.,0.));
#7575=DIRECTION('ref_axis',(0.,0.,1.));
#7576=DIRECTION('center_axis',(0.,-1.,0.));
#7577=DIRECTION('ref_axis',(1.,0.,0.));
#7578=DIRECTION('center_axis',(0.,-1.,0.));
#7579=DIRECTION('ref_axis',(1.,0.,0.));
#7580=DIRECTION('center_axis',(0.,-1.,0.));
#7581=DIRECTION('ref_axis',(1.,0.,0.));
#7582=DIRECTION('center_axis',(0.,-1.,0.));
#7583=DIRECTION('ref_axis',(1.,0.,0.));
#7584=DIRECTION('',(0.,1.,0.));
#7585=DIRECTION('center_axis',(0.,-1.,0.));
#7586=DIRECTION('ref_axis',(0.,0.,-1.));
#7587=DIRECTION('center_axis',(0.,-1.,0.));
#7588=DIRECTION('ref_axis',(1.,0.,0.));
#7589=DIRECTION('center_axis',(0.,-1.,0.));
#7590=DIRECTION('ref_axis',(1.,0.,0.));
#7591=DIRECTION('',(0.,1.,0.));
#7592=DIRECTION('',(0.,0.,1.));
#7593=DIRECTION('',(1.,0.,0.));
#7594=DIRECTION('',(0.,0.,1.));
#7595=DIRECTION('',(1.,0.,0.));
#7596=DIRECTION('',(0.,0.,1.));
#7597=DIRECTION('',(1.,0.,0.));
#7598=DIRECTION('',(0.,0.,1.));
#7599=DIRECTION('',(1.,0.,0.));
#7600=DIRECTION('',(0.,0.,1.));
#7601=DIRECTION('',(1.,0.,0.));
#7602=DIRECTION('axis',(0.,0.,1.));
#7603=DIRECTION('refdir',(1.,0.,0.));
#7604=DIRECTION('axis',(0.,0.,1.));
#7605=DIRECTION('refdir',(1.,0.,0.));
#7606=DIRECTION('center_axis',(0.,0.,1.));
#7607=DIRECTION('ref_axis',(1.,0.,0.));
#7608=DIRECTION('center_axis',(0.,0.,1.));
#7609=DIRECTION('ref_axis',(1.,0.,0.));
#7610=DIRECTION('',(0.,0.,1.));
#7611=DIRECTION('center_axis',(0.,0.,-1.));
#7612=DIRECTION('ref_axis',(1.,0.,0.));
#7613=DIRECTION('center_axis',(0.,0.,1.));
#7614=DIRECTION('ref_axis',(1.,0.,0.));
#7615=DIRECTION('center_axis',(0.,0.,1.));
#7616=DIRECTION('ref_axis',(1.,0.,0.));
#7617=DIRECTION('center_axis',(0.,0.,1.));
#7618=DIRECTION('ref_axis',(1.,0.,0.));
#7619=DIRECTION('',(0.,0.,1.));
#7620=DIRECTION('center_axis',(0.,0.,-1.));
#7621=DIRECTION('ref_axis',(1.,0.,0.));
#7622=DIRECTION('center_axis',(0.,0.,1.));
#7623=DIRECTION('ref_axis',(1.,0.,0.));
#7624=DIRECTION('',(0.,0.,1.));
#7625=DIRECTION('center_axis',(0.,0.,1.));
#7626=DIRECTION('ref_axis',(1.,0.,0.));
#7627=DIRECTION('',(0.,0.,1.));
#7628=DIRECTION('center_axis',(0.,0.,1.));
#7629=DIRECTION('ref_axis',(1.,0.,0.));
#7630=DIRECTION('center_axis',(0.,0.,1.));
#7631=DIRECTION('ref_axis',(1.,0.,0.));
#7632=DIRECTION('',(1.,0.,0.));
#7633=DIRECTION('center_axis',(0.,0.,1.));
#7634=DIRECTION('ref_axis',(1.,0.,0.));
#7635=DIRECTION('',(1.,0.,0.));
#7636=DIRECTION('',(0.,-1.,0.));
#7637=DIRECTION('',(-1.,0.,0.));
#7638=DIRECTION('center_axis',(0.,0.,1.));
#7639=DIRECTION('ref_axis',(1.,0.,0.));
#7640=DIRECTION('',(-1.,0.,0.));
#7641=DIRECTION('center_axis',(0.,0.,1.));
#7642=DIRECTION('ref_axis',(1.,0.,0.));
#7643=DIRECTION('center_axis',(0.,1.,0.));
#7644=DIRECTION('ref_axis',(-1.,0.,0.));
#7645=DIRECTION('',(0.,0.,-1.));
#7646=DIRECTION('',(-1.,0.,0.));
#7647=DIRECTION('center_axis',(0.,-1.,0.));
#7648=DIRECTION('ref_axis',(1.,0.,0.));
#7649=DIRECTION('',(0.,0.,1.));
#7650=DIRECTION('',(1.,0.,0.));
#7651=DIRECTION('center_axis',(0.,-1.,0.));
#7652=DIRECTION('ref_axis',(1.,0.,0.));
#7653=DIRECTION('',(0.,0.,-1.));
#7654=DIRECTION('',(1.,0.,0.));
#7655=DIRECTION('',(0.,0.,1.));
#7656=DIRECTION('center_axis',(0.,1.,0.));
#7657=DIRECTION('ref_axis',(-1.,0.,0.));
#7658=DIRECTION('',(0.,0.,1.));
#7659=DIRECTION('',(0.,0.,1.));
#7660=DIRECTION('',(-1.,0.,0.));
#7661=DIRECTION('center_axis',(-1.,0.,0.));
#7662=DIRECTION('ref_axis',(0.,-1.,0.));
#7663=DIRECTION('',(0.,-1.,0.));
#7664=DIRECTION('center_axis',(0.,0.,1.));
#7665=DIRECTION('ref_axis',(1.,0.,0.));
#7666=DIRECTION('center_axis',(0.,0.,1.));
#7667=DIRECTION('ref_axis',(1.,0.,0.));
#7668=DIRECTION('center_axis',(0.,0.,1.));
#7669=DIRECTION('ref_axis',(1.,0.,0.));
#7670=DIRECTION('center_axis',(0.,0.,1.));
#7671=DIRECTION('ref_axis',(1.,0.,0.));
#7672=DIRECTION('center_axis',(0.,0.,1.));
#7673=DIRECTION('ref_axis',(1.,0.,0.));
#7674=DIRECTION('center_axis',(0.,0.,1.));
#7675=DIRECTION('ref_axis',(1.,0.,0.));
#7676=DIRECTION('center_axis',(0.,0.,1.));
#7677=DIRECTION('ref_axis',(1.,0.,0.));
#7678=DIRECTION('center_axis',(0.,0.,1.));
#7679=DIRECTION('ref_axis',(1.,0.,0.));
#7680=DIRECTION('center_axis',(0.,0.,-1.));
#7681=DIRECTION('ref_axis',(1.,0.,0.));
#7682=DIRECTION('center_axis',(0.,0.,1.));
#7683=DIRECTION('ref_axis',(1.,0.,0.));
#7684=DIRECTION('',(0.,0.,-1.));
#7685=DIRECTION('center_axis',(0.,0.,1.));
#7686=DIRECTION('ref_axis',(1.,0.,0.));
#7687=DIRECTION('',(0.,0.,-1.));
#7688=DIRECTION('center_axis',(0.,0.,1.));
#7689=DIRECTION('ref_axis',(1.,0.,0.));
#7690=DIRECTION('center_axis',(0.,0.,1.));
#7691=DIRECTION('ref_axis',(1.,0.,0.));
#7692=DIRECTION('center_axis',(0.,0.,1.));
#7693=DIRECTION('ref_axis',(1.,0.,0.));
#7694=DIRECTION('',(0.,0.,-1.));
#7695=DIRECTION('center_axis',(0.,0.,1.));
#7696=DIRECTION('ref_axis',(1.,0.,0.));
#7697=DIRECTION('center_axis',(0.,0.,1.));
#7698=DIRECTION('ref_axis',(1.,0.,0.));
#7699=DIRECTION('axis',(0.,0.,1.));
#7700=DIRECTION('refdir',(1.,0.,0.));
#7701=DIRECTION('center_axis',(0.,0.,1.));
#7702=DIRECTION('ref_axis',(1.,0.,0.));
#7703=DIRECTION('center_axis',(0.,0.,-1.));
#7704=DIRECTION('ref_axis',(1.,0.,0.));
#7705=DIRECTION('',(0.,0.,-1.));
#7706=DIRECTION('center_axis',(0.,0.,-1.));
#7707=DIRECTION('ref_axis',(1.,0.,0.));
#7708=DIRECTION('center_axis',(0.,0.,1.));
#7709=DIRECTION('ref_axis',(1.,0.,0.));
#7710=DIRECTION('center_axis',(0.,0.,1.));
#7711=DIRECTION('ref_axis',(1.,0.,0.));
#7712=DIRECTION('',(0.,0.,-1.));
#7713=DIRECTION('center_axis',(0.,0.,1.));
#7714=DIRECTION('ref_axis',(1.,0.,0.));
#7715=DIRECTION('center_axis',(0.,0.,1.));
#7716=DIRECTION('ref_axis',(1.,0.,0.));
#7717=DIRECTION('center_axis',(0.,0.,1.));
#7718=DIRECTION('ref_axis',(1.,0.,0.));
#7719=DIRECTION('axis',(0.,0.,1.));
#7720=DIRECTION('refdir',(1.,0.,0.));
#7721=DIRECTION('center_axis',(0.,1.,0.));
#7722=DIRECTION('ref_axis',(1.,0.,0.));
#7723=DIRECTION('',(0.,0.,-1.));
#7724=DIRECTION('center_axis',(0.,1.,0.));
#7725=DIRECTION('ref_axis',(1.,0.,0.));
#7726=DIRECTION('center_axis',(0.,1.,0.));
#7727=DIRECTION('ref_axis',(1.,0.,0.));
#7728=DIRECTION('center_axis',(0.,1.,0.));
#7729=DIRECTION('ref_axis',(1.,0.,0.));
#7730=DIRECTION('',(0.,1.,0.));
#7731=DIRECTION('center_axis',(0.,1.,0.));
#7732=DIRECTION('ref_axis',(1.,0.,0.));
#7733=DIRECTION('center_axis',(0.,1.,0.));
#7734=DIRECTION('ref_axis',(1.,0.,0.));
#7735=DIRECTION('',(0.,0.,1.));
#7736=DIRECTION('center_axis',(1.,0.,0.));
#7737=DIRECTION('ref_axis',(0.,0.,-1.));
#7738=DIRECTION('',(0.,0.,-1.));
#7739=DIRECTION('center_axis',(1.,0.,0.));
#7740=DIRECTION('ref_axis',(0.,0.,-1.));
#7741=DIRECTION('center_axis',(1.,0.,0.));
#7742=DIRECTION('ref_axis',(0.,0.,-1.));
#7743=DIRECTION('',(1.,0.,0.));
#7744=DIRECTION('center_axis',(1.,0.,0.));
#7745=DIRECTION('ref_axis',(0.,0.,-1.));
#7746=DIRECTION('center_axis',(1.,0.,0.));
#7747=DIRECTION('ref_axis',(0.,0.,-1.));
#7748=DIRECTION('',(0.,0.,1.));
#7749=DIRECTION('center_axis',(0.,0.,1.));
#7750=DIRECTION('ref_axis',(1.,0.,0.));
#7751=DIRECTION('center_axis',(0.,0.,-1.));
#7752=DIRECTION('ref_axis',(1.,0.,0.));
#7753=DIRECTION('',(0.,0.,-1.));
#7754=DIRECTION('',(0.,0.,-1.));
#7755=DIRECTION('center_axis',(0.,0.,-1.));
#7756=DIRECTION('ref_axis',(1.,0.,0.));
#7757=DIRECTION('center_axis',(0.,0.,1.));
#7758=DIRECTION('ref_axis',(1.,0.,0.));
#7759=DIRECTION('center_axis',(0.,0.,1.));
#7760=DIRECTION('ref_axis',(1.,0.,0.));
#7761=DIRECTION('',(0.,0.,-1.));
#7762=DIRECTION('',(0.,0.,-1.));
#7763=DIRECTION('center_axis',(0.,0.,1.));
#7764=DIRECTION('ref_axis',(1.,0.,0.));
#7765=DIRECTION('center_axis',(0.,0.,1.));
#7766=DIRECTION('ref_axis',(1.,0.,0.));
#7767=DIRECTION('center_axis',(0.,0.,1.));
#7768=DIRECTION('ref_axis',(1.,0.,0.));
#7769=DIRECTION('axis',(0.,0.,1.));
#7770=DIRECTION('refdir',(1.,0.,0.));
#7771=DIRECTION('center_axis',(0.,0.,1.));
#7772=DIRECTION('ref_axis',(1.,0.,0.));
#7773=DIRECTION('center_axis',(0.,0.,1.));
#7774=DIRECTION('ref_axis',(1.,0.,0.));
#7775=DIRECTION('center_axis',(0.,0.,1.));
#7776=DIRECTION('ref_axis',(1.,0.,0.));
#7777=DIRECTION('center_axis',(0.,0.,1.));
#7778=DIRECTION('ref_axis',(1.,0.,0.));
#7779=DIRECTION('center_axis',(0.,0.,1.));
#7780=DIRECTION('ref_axis',(1.,0.,0.));
#7781=DIRECTION('center_axis',(0.,0.,-1.));
#7782=DIRECTION('ref_axis',(1.,0.,0.));
#7783=DIRECTION('center_axis',(0.,0.,1.));
#7784=DIRECTION('ref_axis',(1.,0.,0.));
#7785=DIRECTION('',(0.,0.,-1.));
#7786=DIRECTION('center_axis',(0.,0.,1.));
#7787=DIRECTION('ref_axis',(1.,0.,0.));
#7788=DIRECTION('',(0.,0.,-1.));
#7789=DIRECTION('center_axis',(0.,0.,1.));
#7790=DIRECTION('ref_axis',(1.,0.,0.));
#7791=DIRECTION('center_axis',(0.,0.,1.));
#7792=DIRECTION('ref_axis',(1.,0.,0.));
#7793=DIRECTION('center_axis',(0.,0.,1.));
#7794=DIRECTION('ref_axis',(1.,0.,0.));
#7795=DIRECTION('',(0.,0.,-1.));
#7796=DIRECTION('center_axis',(0.,0.,1.));
#7797=DIRECTION('ref_axis',(1.,0.,0.));
#7798=DIRECTION('center_axis',(0.,0.,1.));
#7799=DIRECTION('ref_axis',(1.,0.,0.));
#7800=DIRECTION('axis',(0.,0.,1.));
#7801=DIRECTION('refdir',(1.,0.,0.));
#7802=DIRECTION('center_axis',(0.,0.,1.));
#7803=DIRECTION('ref_axis',(1.,0.,0.));
#7804=DIRECTION('center_axis',(0.,0.,1.));
#7805=DIRECTION('ref_axis',(1.,0.,0.));
#7806=DIRECTION('',(0.,0.,1.));
#7807=DIRECTION('center_axis',(0.,0.,-1.));
#7808=DIRECTION('ref_axis',(1.,0.,0.));
#7809=DIRECTION('center_axis',(0.,0.,1.));
#7810=DIRECTION('ref_axis',(1.,0.,0.));
#7811=DIRECTION('',(0.,0.,-1.));
#7812=DIRECTION('center_axis',(0.,0.,1.));
#7813=DIRECTION('ref_axis',(1.,0.,0.));
#7814=DIRECTION('',(0.,0.,1.));
#7815=DIRECTION('center_axis',(0.,0.,1.));
#7816=DIRECTION('ref_axis',(1.,0.,0.));
#7817=DIRECTION('center_axis',(0.,0.,1.));
#7818=DIRECTION('ref_axis',(1.,0.,0.));
#7819=DIRECTION('',(0.,-1.,0.));
#7820=DIRECTION('center_axis',(0.,0.,1.));
#7821=DIRECTION('ref_axis',(1.,0.,0.));
#7822=DIRECTION('',(0.,-1.,0.));
#7823=DIRECTION('center_axis',(-1.,0.,0.));
#7824=DIRECTION('ref_axis',(0.,-1.,0.));
#7825=DIRECTION('',(0.,1.,0.));
#7826=DIRECTION('',(0.,0.,1.));
#7827=DIRECTION('center_axis',(-1.,0.,0.));
#7828=DIRECTION('ref_axis',(0.,-1.,0.));
#7829=DIRECTION('',(0.,0.,-1.));
#7830=DIRECTION('',(0.,1.,0.));
#7831=DIRECTION('center_axis',(0.,0.,1.));
#7832=DIRECTION('ref_axis',(-1.,1.22464679914735E-16,0.));
#7833=DIRECTION('center_axis',(0.,0.,1.));
#7834=DIRECTION('ref_axis',(1.,0.,0.));
#7835=DIRECTION('center_axis',(0.,0.,1.));
#7836=DIRECTION('ref_axis',(1.,0.,0.));
#7837=DIRECTION('axis',(0.,0.,1.));
#7838=DIRECTION('refdir',(1.,0.,0.));
#7839=DIRECTION('center_axis',(0.,0.,1.));
#7840=DIRECTION('ref_axis',(1.,0.,0.));
#7841=DIRECTION('center_axis',(0.,0.,-1.));
#7842=DIRECTION('ref_axis',(1.,0.,0.));
#7843=DIRECTION('',(0.,0.,-1.));
#7844=DIRECTION('center_axis',(0.,0.,-1.));
#7845=DIRECTION('ref_axis',(1.,0.,0.));
#7846=DIRECTION('center_axis',(0.,0.,1.));
#7847=DIRECTION('ref_axis',(1.,0.,0.));
#7848=DIRECTION('center_axis',(0.,0.,1.));
#7849=DIRECTION('ref_axis',(1.,0.,0.));
#7850=DIRECTION('',(0.,0.,-1.));
#7851=DIRECTION('center_axis',(0.,0.,1.));
#7852=DIRECTION('ref_axis',(1.,0.,0.));
#7853=DIRECTION('center_axis',(0.,0.,1.));
#7854=DIRECTION('ref_axis',(1.,0.,0.));
#7855=DIRECTION('center_axis',(0.,0.,1.));
#7856=DIRECTION('ref_axis',(1.,0.,0.));
#7857=DIRECTION('axis',(0.,0.,1.));
#7858=DIRECTION('refdir',(1.,0.,0.));
#7859=DIRECTION('center_axis',(0.,0.,1.));
#7860=DIRECTION('ref_axis',(1.,0.,0.));
#7861=DIRECTION('center_axis',(0.,0.,-1.));
#7862=DIRECTION('ref_axis',(1.,0.,0.));
#7863=DIRECTION('',(0.,0.,-1.));
#7864=DIRECTION('center_axis',(0.,0.,-1.));
#7865=DIRECTION('ref_axis',(1.,0.,0.));
#7866=DIRECTION('center_axis',(0.,0.,1.));
#7867=DIRECTION('ref_axis',(1.,0.,0.));
#7868=DIRECTION('center_axis',(0.,0.,1.));
#7869=DIRECTION('ref_axis',(1.,0.,0.));
#7870=DIRECTION('',(0.,0.,-1.));
#7871=DIRECTION('center_axis',(0.,0.,1.));
#7872=DIRECTION('ref_axis',(1.,0.,0.));
#7873=DIRECTION('center_axis',(0.,0.,1.));
#7874=DIRECTION('ref_axis',(1.,0.,0.));
#7875=DIRECTION('center_axis',(0.,0.,1.));
#7876=DIRECTION('ref_axis',(1.,0.,0.));
#7877=DIRECTION('axis',(0.,0.,1.));
#7878=DIRECTION('refdir',(1.,0.,0.));
#7879=DIRECTION('center_axis',(0.,0.,1.));
#7880=DIRECTION('ref_axis',(1.,0.,0.));
#7881=DIRECTION('center_axis',(0.,0.,-1.));
#7882=DIRECTION('ref_axis',(1.,0.,0.));
#7883=DIRECTION('',(0.,0.,-1.));
#7884=DIRECTION('center_axis',(0.,0.,-1.));
#7885=DIRECTION('ref_axis',(1.,0.,0.));
#7886=DIRECTION('center_axis',(0.,0.,1.));
#7887=DIRECTION('ref_axis',(1.,0.,0.));
#7888=DIRECTION('center_axis',(0.,0.,1.));
#7889=DIRECTION('ref_axis',(1.,0.,0.));
#7890=DIRECTION('',(0.,0.,-1.));
#7891=DIRECTION('center_axis',(0.,0.,1.));
#7892=DIRECTION('ref_axis',(1.,0.,0.));
#7893=DIRECTION('center_axis',(0.,0.,1.));
#7894=DIRECTION('ref_axis',(1.,0.,0.));
#7895=DIRECTION('center_axis',(0.,0.,1.));
#7896=DIRECTION('ref_axis',(1.,0.,0.));
#7897=DIRECTION('axis',(0.,0.,1.));
#7898=DIRECTION('refdir',(1.,0.,0.));
#7899=DIRECTION('center_axis',(0.866025403784439,0.,-0.5));
#7900=DIRECTION('ref_axis',(0.5,0.,0.866025403784439));
#7901=DIRECTION('',(-0.5,0.,-0.866025403784439));
#7902=DIRECTION('',(0.,-1.,0.));
#7903=DIRECTION('',(0.5,0.,0.866025403784439));
#7904=DIRECTION('',(0.,-1.,0.));
#7905=DIRECTION('center_axis',(1.60246890531964E-16,0.,-1.));
#7906=DIRECTION('ref_axis',(1.,0.,1.60246890531964E-16));
#7907=DIRECTION('',(-1.,0.,-1.60246890531964E-16));
#7908=DIRECTION('',(0.,-1.,0.));
#7909=DIRECTION('',(1.,0.,1.60246890531964E-16));
#7910=DIRECTION('center_axis',(-0.866025403784439,0.,-0.5));
#7911=DIRECTION('ref_axis',(0.5,0.,-0.866025403784439));
#7912=DIRECTION('',(-0.5,0.,0.866025403784439));
#7913=DIRECTION('',(0.,-1.,0.));
#7914=DIRECTION('',(0.5,0.,-0.866025403784439));
#7915=DIRECTION('center_axis',(-0.866025403784439,0.,0.5));
#7916=DIRECTION('ref_axis',(-0.5,0.,-0.866025403784439));
#7917=DIRECTION('',(0.5,0.,0.866025403784439));
#7918=DIRECTION('',(0.,-1.,0.));
#7919=DIRECTION('',(-0.5,0.,-0.866025403784439));
#7920=DIRECTION('center_axis',(-1.60246890531964E-16,0.,1.));
#7921=DIRECTION('ref_axis',(-1.,0.,-1.60246890531964E-16));
#7922=DIRECTION('',(1.,0.,1.60246890531964E-16));
#7923=DIRECTION('',(0.,-1.,0.));
#7924=DIRECTION('',(-1.,0.,-1.60246890531964E-16));
#7925=DIRECTION('center_axis',(0.866025403784439,0.,0.5));
#7926=DIRECTION('ref_axis',(-0.5,0.,0.866025403784439));
#7927=DIRECTION('',(0.5,0.,-0.866025403784439));
#7928=DIRECTION('',(-0.5,0.,0.866025403784439));
#7929=DIRECTION('center_axis',(0.,1.,0.));
#7930=DIRECTION('ref_axis',(1.,0.,0.));
#7931=DIRECTION('center_axis',(0.,-1.,0.));
#7932=DIRECTION('ref_axis',(0.,0.,-1.));
#7933=DIRECTION('center_axis',(0.,1.,0.));
#7934=DIRECTION('ref_axis',(1.,0.,0.));
#7935=DIRECTION('center_axis',(0.,1.,0.));
#7936=DIRECTION('ref_axis',(1.,0.,0.));
#7937=DIRECTION('center_axis',(0.,1.,0.));
#7938=DIRECTION('ref_axis',(0.,0.,1.));
#7939=DIRECTION('center_axis',(0.,-1.,0.));
#7940=DIRECTION('ref_axis',(1.,0.,0.));
#7941=DIRECTION('center_axis',(0.,-1.,0.));
#7942=DIRECTION('ref_axis',(1.,0.,0.));
#7943=DIRECTION('center_axis',(0.,-1.,0.));
#7944=DIRECTION('ref_axis',(1.,0.,0.));
#7945=DIRECTION('',(0.707106781186547,0.707106781186548,8.65956056235493E-17));
#7946=DIRECTION('center_axis',(0.,-1.,0.));
#7947=DIRECTION('ref_axis',(1.,0.,0.));
#7948=DIRECTION('center_axis',(0.,-1.,0.));
#7949=DIRECTION('ref_axis',(1.,0.,0.));
#7950=DIRECTION('',(0.,1.,0.));
#7951=DIRECTION('center_axis',(0.,1.,0.));
#7952=DIRECTION('ref_axis',(1.,0.,0.));
#7953=DIRECTION('center_axis',(0.,-1.,0.));
#7954=DIRECTION('ref_axis',(1.,0.,0.));
#7955=DIRECTION('',(-0.707106781186547,0.707106781186548,-8.65956056235493E-17));
#7956=DIRECTION('center_axis',(0.,-1.,0.));
#7957=DIRECTION('ref_axis',(0.,0.,-1.));
#7958=DIRECTION('center_axis',(0.,-1.,0.));
#7959=DIRECTION('ref_axis',(1.,0.,0.));
#7960=DIRECTION('center_axis',(0.,1.,0.));
#7961=DIRECTION('ref_axis',(1.,0.,0.));
#7962=DIRECTION('center_axis',(0.,1.,0.));
#7963=DIRECTION('ref_axis',(1.,0.,0.));
#7964=DIRECTION('',(-0.447213595499958,0.894427190999916,-5.47678698264203E-17));
#7965=DIRECTION('center_axis',(0.,-1.,0.));
#7966=DIRECTION('ref_axis',(1.,0.,0.));
#7967=DIRECTION('',(0.,1.,0.));
#7968=DIRECTION('',(0.,0.,1.));
#7969=DIRECTION('',(1.,0.,0.));
#7970=DIRECTION('',(0.,0.,1.));
#7971=DIRECTION('',(1.,0.,0.));
#7972=DIRECTION('',(0.,0.,1.));
#7973=DIRECTION('',(1.,0.,0.));
#7974=DIRECTION('',(0.,0.,1.));
#7975=DIRECTION('',(1.,0.,0.));
#7976=DIRECTION('',(0.,0.,1.));
#7977=DIRECTION('',(1.,0.,0.));
#7978=DIRECTION('',(0.,-1.,2.22044604925031E-16));
#7979=DIRECTION('',(1.,0.,0.));
#7980=DIRECTION('',(0.,-1.,2.22044604925031E-16));
#7981=DIRECTION('',(1.,0.,0.));
#7982=DIRECTION('',(0.,-1.,2.22044604925031E-16));
#7983=DIRECTION('',(1.,0.,0.));
#7984=DIRECTION('',(0.,-1.,2.22044604925031E-16));
#7985=DIRECTION('',(1.,0.,0.));
#7986=DIRECTION('',(0.,-1.,2.22044604925031E-16));
#7987=DIRECTION('',(1.,0.,0.));
#7988=DIRECTION('',(0.,-1.,2.22044604925031E-16));
#7989=DIRECTION('',(1.,0.,0.));
#7990=DIRECTION('',(0.,-1.,2.22044604925031E-16));
#7991=DIRECTION('',(1.,0.,0.));
#7992=DIRECTION('',(0.,-1.,2.22044604925031E-16));
#7993=DIRECTION('',(1.,0.,0.));
#7994=DIRECTION('',(0.,-1.,2.22044604925031E-16));
#7995=DIRECTION('',(1.,0.,0.));
#7996=DIRECTION('',(0.,-1.,2.22044604925031E-16));
#7997=DIRECTION('',(1.,0.,0.));
#7998=DIRECTION('',(0.,-1.,2.22044604925031E-16));
#7999=DIRECTION('',(1.,0.,0.));
#8000=DIRECTION('',(0.,-1.,2.22044604925031E-16));
#8001=DIRECTION('',(1.,0.,0.));
#8002=DIRECTION('',(0.,-1.,2.22044604925031E-16));
#8003=DIRECTION('',(1.,0.,0.));
#8004=DIRECTION('',(0.,-1.,2.22044604925031E-16));
#8005=DIRECTION('',(1.,0.,0.));
#8006=DIRECTION('axis',(0.,0.,1.));
#8007=DIRECTION('refdir',(1.,0.,0.));
#8008=DIRECTION('axis',(0.,0.,1.));
#8009=DIRECTION('refdir',(1.,0.,0.));
#8010=DIRECTION('center_axis',(0.,0.,1.));
#8011=DIRECTION('ref_axis',(1.,0.,0.));
#8012=DIRECTION('center_axis',(0.,0.,1.));
#8013=DIRECTION('ref_axis',(1.,0.,0.));
#8014=DIRECTION('',(0.,0.,1.));
#8015=DIRECTION('center_axis',(0.,0.,-1.));
#8016=DIRECTION('ref_axis',(1.,0.,0.));
#8017=DIRECTION('center_axis',(0.,0.,1.));
#8018=DIRECTION('ref_axis',(1.,0.,0.));
#8019=DIRECTION('center_axis',(0.,0.,1.));
#8020=DIRECTION('ref_axis',(1.,0.,0.));
#8021=DIRECTION('',(0.,0.,1.));
#8022=DIRECTION('center_axis',(0.,0.,-1.));
#8023=DIRECTION('ref_axis',(1.,0.,0.));
#8024=DIRECTION('center_axis',(0.,0.,1.));
#8025=DIRECTION('ref_axis',(1.,0.,0.));
#8026=DIRECTION('center_axis',(0.,0.,1.));
#8027=DIRECTION('ref_axis',(1.,0.,0.));
#8028=DIRECTION('',(0.,0.,1.));
#8029=DIRECTION('center_axis',(0.,0.,-1.));
#8030=DIRECTION('ref_axis',(1.,0.,0.));
#8031=DIRECTION('center_axis',(0.,0.,1.));
#8032=DIRECTION('ref_axis',(1.,0.,0.));
#8033=DIRECTION('center_axis',(0.,0.,1.));
#8034=DIRECTION('ref_axis',(1.,0.,0.));
#8035=DIRECTION('',(0.,0.,1.));
#8036=DIRECTION('center_axis',(0.,0.,-1.));
#8037=DIRECTION('ref_axis',(1.,0.,0.));
#8038=DIRECTION('center_axis',(0.,0.,1.));
#8039=DIRECTION('ref_axis',(1.,0.,0.));
#8040=DIRECTION('center_axis',(0.,0.,1.));
#8041=DIRECTION('ref_axis',(1.,0.,0.));
#8042=DIRECTION('',(0.,0.,-1.));
#8043=DIRECTION('center_axis',(0.,0.,-1.));
#8044=DIRECTION('ref_axis',(1.,0.,0.));
#8045=DIRECTION('',(0.,0.,1.));
#8046=DIRECTION('center_axis',(0.,0.,1.));
#8047=DIRECTION('ref_axis',(1.,0.,0.));
#8048=DIRECTION('center_axis',(0.,0.,1.));
#8049=DIRECTION('ref_axis',(1.,0.,0.));
#8050=DIRECTION('',(0.,0.,-1.));
#8051=DIRECTION('center_axis',(0.,0.,-1.));
#8052=DIRECTION('ref_axis',(1.,0.,0.));
#8053=DIRECTION('',(0.,0.,1.));
#8054=DIRECTION('center_axis',(0.,0.,1.));
#8055=DIRECTION('ref_axis',(1.,0.,0.));
#8056=DIRECTION('center_axis',(0.,0.,1.));
#8057=DIRECTION('ref_axis',(1.,0.,0.));
#8058=DIRECTION('',(0.,0.,-1.));
#8059=DIRECTION('center_axis',(0.,0.,-1.));
#8060=DIRECTION('ref_axis',(1.,0.,0.));
#8061=DIRECTION('',(0.,0.,1.));
#8062=DIRECTION('center_axis',(0.,0.,1.));
#8063=DIRECTION('ref_axis',(1.,0.,0.));
#8064=DIRECTION('',(0.,0.,-1.));
#8065=DIRECTION('center_axis',(0.,0.,-1.));
#8066=DIRECTION('ref_axis',(1.,0.,0.));
#8067=DIRECTION('',(0.,0.,1.));
#8068=DIRECTION('center_axis',(0.,0.,1.));
#8069=DIRECTION('ref_axis',(1.,0.,0.));
#8070=DIRECTION('center_axis',(0.,0.,1.));
#8071=DIRECTION('ref_axis',(1.,0.,0.));
#8072=DIRECTION('center_axis',(0.,0.,1.));
#8073=DIRECTION('ref_axis',(1.,0.,0.));
#8074=DIRECTION('',(0.,0.,1.));
#8075=DIRECTION('center_axis',(0.,0.,1.));
#8076=DIRECTION('ref_axis',(1.,0.,0.));
#8077=DIRECTION('center_axis',(0.,0.,1.));
#8078=DIRECTION('ref_axis',(1.,0.,0.));
#8079=DIRECTION('center_axis',(0.,0.,1.));
#8080=DIRECTION('ref_axis',(1.,0.,0.));
#8081=DIRECTION('',(0.,0.,1.));
#8082=DIRECTION('center_axis',(0.,0.,1.));
#8083=DIRECTION('ref_axis',(1.,0.,0.));
#8084=DIRECTION('center_axis',(0.,0.,1.));
#8085=DIRECTION('ref_axis',(1.,0.,0.));
#8086=DIRECTION('center_axis',(0.,0.,1.));
#8087=DIRECTION('ref_axis',(1.,0.,0.));
#8088=DIRECTION('',(0.,0.,1.));
#8089=DIRECTION('center_axis',(0.,0.,1.));
#8090=DIRECTION('ref_axis',(1.,0.,0.));
#8091=DIRECTION('center_axis',(0.,0.,1.));
#8092=DIRECTION('ref_axis',(1.,0.,0.));
#8093=DIRECTION('',(0.,1.,0.));
#8094=DIRECTION('',(1.,0.,0.));
#8095=DIRECTION('',(1.70803542250024E-16,1.,0.));
#8096=DIRECTION('center_axis',(0.,0.,-1.));
#8097=DIRECTION('ref_axis',(1.,0.,0.));
#8098=DIRECTION('',(-3.41607084500048E-16,-1.,0.));
#8099=DIRECTION('',(1.,0.,0.));
#8100=DIRECTION('',(0.,-1.,0.));
#8101=DIRECTION('center_axis',(0.,0.,1.));
#8102=DIRECTION('ref_axis',(1.,0.,0.));
#8103=DIRECTION('center_axis',(0.,0.,1.));
#8104=DIRECTION('ref_axis',(1.,0.,0.));
#8105=DIRECTION('',(-1.,0.,0.));
#8106=DIRECTION('',(0.,1.,0.));
#8107=DIRECTION('',(-1.,0.,0.));
#8108=DIRECTION('center_axis',(0.,0.,-1.));
#8109=DIRECTION('ref_axis',(1.,0.,0.));
#8110=DIRECTION('',(1.,0.,0.));
#8111=DIRECTION('',(0.,1.,0.));
#8112=DIRECTION('',(1.,0.,0.));
#8113=DIRECTION('center_axis',(0.,0.,1.));
#8114=DIRECTION('ref_axis',(1.,0.,0.));
#8115=DIRECTION('',(0.,-1.,0.));
#8116=DIRECTION('',(-1.,0.,0.));
#8117=DIRECTION('',(0.,-1.,0.));
#8118=DIRECTION('center_axis',(0.,0.,-1.));
#8119=DIRECTION('ref_axis',(1.,0.,0.));
#8120=DIRECTION('',(0.,1.,0.));
#8121=DIRECTION('',(-1.,0.,0.));
#8122=DIRECTION('',(0.,1.,0.));
#8123=DIRECTION('center_axis',(0.,0.,1.));
#8124=DIRECTION('ref_axis',(1.,0.,0.));
#8125=DIRECTION('',(1.,-1.11022302462516E-16,0.));
#8126=DIRECTION('',(0.,-1.,0.));
#8127=DIRECTION('',(1.,-1.06752213906265E-16,0.));
#8128=DIRECTION('center_axis',(0.,0.,-1.));
#8129=DIRECTION('ref_axis',(1.,0.,0.));
#8130=DIRECTION('',(-1.,1.28102656687518E-16,0.));
#8131=DIRECTION('',(0.,-1.,0.));
#8132=DIRECTION('',(-1.,5.55111512312578E-17,0.));
#8133=DIRECTION('center_axis',(0.,0.,1.));
#8134=DIRECTION('ref_axis',(1.,0.,0.));
#8135=DIRECTION('center_axis',(0.,0.,1.));
#8136=DIRECTION('ref_axis',(1.,0.,0.));
#8137=DIRECTION('center_axis',(0.,0.,1.));
#8138=DIRECTION('ref_axis',(1.,0.,0.));
#8139=DIRECTION('',(0.,0.,1.));
#8140=DIRECTION('center_axis',(0.,0.,1.));
#8141=DIRECTION('ref_axis',(1.,0.,0.));
#8142=DIRECTION('',(0.,0.,-1.));
#8143=DIRECTION('center_axis',(0.,0.,1.));
#8144=DIRECTION('ref_axis',(1.,0.,0.));
#8145=DIRECTION('center_axis',(1.,0.,0.));
#8146=DIRECTION('ref_axis',(0.,1.,0.));
#8147=DIRECTION('',(0.,0.,1.));
#8148=DIRECTION('',(0.,1.,0.));
#8149=DIRECTION('center_axis',(0.,1.,0.));
#8150=DIRECTION('ref_axis',(-1.,0.,0.));
#8151=DIRECTION('',(0.,0.,1.));
#8152=DIRECTION('',(-1.,0.,0.));
#8153=DIRECTION('center_axis',(0.,1.,0.));
#8154=DIRECTION('ref_axis',(-1.,0.,0.));
#8155=DIRECTION('',(0.,0.,1.));
#8156=DIRECTION('',(-1.,0.,0.));
#8157=DIRECTION('',(0.,0.,-1.));
#8158=DIRECTION('center_axis',(-1.,0.,0.));
#8159=DIRECTION('ref_axis',(0.,-1.,0.));
#8160=DIRECTION('',(0.,-1.,0.));
#8161=DIRECTION('center_axis',(-1.,1.70803542250024E-16,0.));
#8162=DIRECTION('ref_axis',(-1.70803542250024E-16,-1.,0.));
#8163=DIRECTION('',(-1.70803542250024E-16,-1.,0.));
#8164=DIRECTION('',(0.,0.,1.));
#8165=DIRECTION('center_axis',(0.,0.,1.));
#8166=DIRECTION('ref_axis',(1.,0.,0.));
#8167=DIRECTION('center_axis',(0.,0.,1.));
#8168=DIRECTION('ref_axis',(1.,0.,0.));
#8169=DIRECTION('',(1.,-5.55111512312578E-17,0.));
#8170=DIRECTION('',(0.,1.,0.));
#8171=DIRECTION('',(1.,-1.28102656687518E-16,0.));
#8172=DIRECTION('center_axis',(0.,0.,1.));
#8173=DIRECTION('ref_axis',(1.,0.,0.));
#8174=DIRECTION('center_axis',(0.,0.,1.));
#8175=DIRECTION('ref_axis',(1.,0.,0.));
#8176=DIRECTION('center_axis',(0.,0.,1.));
#8177=DIRECTION('ref_axis',(1.,0.,0.));
#8178=DIRECTION('center_axis',(0.,0.,1.));
#8179=DIRECTION('ref_axis',(1.,0.,0.));
#8180=DIRECTION('',(3.41607084500048E-16,1.,0.));
#8181=DIRECTION('center_axis',(0.,0.,1.));
#8182=DIRECTION('ref_axis',(1.,0.,0.));
#8183=DIRECTION('center_axis',(0.,0.,1.));
#8184=DIRECTION('ref_axis',(1.,0.,0.));
#8185=DIRECTION('center_axis',(0.,0.,1.));
#8186=DIRECTION('ref_axis',(1.,0.,0.));
#8187=DIRECTION('',(1.,0.,0.));
#8188=DIRECTION('',(0.,-1.,0.));
#8189=DIRECTION('',(1.,0.,0.));
#8190=DIRECTION('center_axis',(0.,0.,1.));
#8191=DIRECTION('ref_axis',(1.,0.,0.));
#8192=DIRECTION('center_axis',(0.,0.,-1.));
#8193=DIRECTION('ref_axis',(1.,0.,0.));
#8194=DIRECTION('center_axis',(0.,0.,1.));
#8195=DIRECTION('ref_axis',(1.,0.,0.));
#8196=DIRECTION('center_axis',(0.,0.,1.));
#8197=DIRECTION('ref_axis',(1.,0.,0.));
#8198=DIRECTION('',(0.,0.,-1.));
#8199=DIRECTION('',(0.,0.,1.));
#8200=DIRECTION('',(0.,0.,1.));
#8201=DIRECTION('center_axis',(0.,0.,1.));
#8202=DIRECTION('ref_axis',(1.,0.,0.));
#8203=DIRECTION('',(0.,0.,-1.));
#8204=DIRECTION('center_axis',(0.,0.,-1.));
#8205=DIRECTION('ref_axis',(1.,0.,0.));
#8206=DIRECTION('',(0.,0.,-1.));
#8207=DIRECTION('center_axis',(0.,0.,1.));
#8208=DIRECTION('ref_axis',(1.,0.,0.));
#8209=DIRECTION('center_axis',(0.,0.,-1.));
#8210=DIRECTION('ref_axis',(1.,0.,0.));
#8211=DIRECTION('',(0.,0.,1.));
#8212=DIRECTION('center_axis',(0.,0.,1.));
#8213=DIRECTION('ref_axis',(1.,0.,0.));
#8214=DIRECTION('',(0.,0.,-1.));
#8215=DIRECTION('center_axis',(0.,0.,-1.));
#8216=DIRECTION('ref_axis',(1.,0.,0.));
#8217=DIRECTION('',(0.,0.,1.));
#8218=DIRECTION('center_axis',(0.,0.,1.));
#8219=DIRECTION('ref_axis',(1.,0.,0.));
#8220=DIRECTION('',(0.,0.,-1.));
#8221=DIRECTION('center_axis',(0.,0.,-1.));
#8222=DIRECTION('ref_axis',(1.,0.,0.));
#8223=DIRECTION('',(0.,0.,1.));
#8224=DIRECTION('center_axis',(1.,-3.41607084500048E-16,0.));
#8225=DIRECTION('ref_axis',(3.41607084500048E-16,1.,0.));
#8226=DIRECTION('center_axis',(0.,0.,1.));
#8227=DIRECTION('ref_axis',(1.,0.,0.));
#8228=DIRECTION('',(0.,0.,-1.));
#8229=DIRECTION('center_axis',(-5.55111512312578E-17,-1.,0.));
#8230=DIRECTION('ref_axis',(1.,-5.55111512312578E-17,0.));
#8231=DIRECTION('',(0.,0.,1.));
#8232=DIRECTION('center_axis',(1.,0.,0.));
#8233=DIRECTION('ref_axis',(0.,1.,0.));
#8234=DIRECTION('',(0.,0.,1.));
#8235=DIRECTION('center_axis',(1.,0.,0.));
#8236=DIRECTION('ref_axis',(0.,1.,0.));
#8237=DIRECTION('',(0.,0.,1.));
#8238=DIRECTION('',(0.,1.,0.));
#8239=DIRECTION('',(0.,0.,-1.));
#8240=DIRECTION('center_axis',(1.11022302462516E-16,1.,0.));
#8241=DIRECTION('ref_axis',(-1.,1.11022302462516E-16,0.));
#8242=DIRECTION('',(-1.,1.11022302462516E-16,0.));
#8243=DIRECTION('center_axis',(1.06752213906265E-16,1.,0.));
#8244=DIRECTION('ref_axis',(-1.,1.06752213906265E-16,0.));
#8245=DIRECTION('',(-1.,1.06752213906265E-16,0.));
#8246=DIRECTION('',(0.,0.,1.));
#8247=DIRECTION('center_axis',(0.,0.,1.));
#8248=DIRECTION('ref_axis',(1.,0.,0.));
#8249=DIRECTION('center_axis',(0.,0.,1.));
#8250=DIRECTION('ref_axis',(1.,0.,0.));
#8251=DIRECTION('',(0.,-1.,0.));
#8252=DIRECTION('',(1.,0.,0.));
#8253=DIRECTION('',(0.,-1.,0.));
#8254=DIRECTION('center_axis',(0.,0.,1.));
#8255=DIRECTION('ref_axis',(1.,0.,0.));
#8256=DIRECTION('center_axis',(0.,0.,1.));
#8257=DIRECTION('ref_axis',(1.,0.,0.));
#8258=DIRECTION('center_axis',(0.,0.,1.));
#8259=DIRECTION('ref_axis',(1.,0.,0.));
#8260=DIRECTION('center_axis',(0.,0.,1.));
#8261=DIRECTION('ref_axis',(1.,0.,0.));
#8262=DIRECTION('center_axis',(0.,0.,1.));
#8263=DIRECTION('ref_axis',(1.,0.,0.));
#8264=DIRECTION('',(0.,0.,1.));
#8265=DIRECTION('center_axis',(-1.28102656687518E-16,-1.,0.));
#8266=DIRECTION('ref_axis',(1.,-1.28102656687518E-16,0.));
#8267=DIRECTION('center_axis',(0.,0.,1.));
#8268=DIRECTION('ref_axis',(1.,0.,0.));
#8269=DIRECTION('',(0.,0.,-1.));
#8270=DIRECTION('center_axis',(-1.,0.,0.));
#8271=DIRECTION('ref_axis',(0.,-1.,0.));
#8272=DIRECTION('',(0.,0.,1.));
#8273=DIRECTION('center_axis',(0.,-1.,0.));
#8274=DIRECTION('ref_axis',(1.,0.,0.));
#8275=DIRECTION('',(0.,0.,1.));
#8276=DIRECTION('center_axis',(0.,-1.,0.));
#8277=DIRECTION('ref_axis',(1.,0.,0.));
#8278=DIRECTION('',(0.,0.,1.));
#8279=DIRECTION('',(1.,0.,0.));
#8280=DIRECTION('',(0.,0.,-1.));
#8281=DIRECTION('center_axis',(1.,0.,0.));
#8282=DIRECTION('ref_axis',(0.,1.,0.));
#8283=DIRECTION('',(0.,1.,0.));
#8284=DIRECTION('center_axis',(1.,0.,0.));
#8285=DIRECTION('ref_axis',(0.,1.,0.));
#8286=DIRECTION('',(0.,1.,0.));
#8287=DIRECTION('',(0.,0.,1.));
#8288=DIRECTION('center_axis',(0.,0.,1.));
#8289=DIRECTION('ref_axis',(1.,0.,0.));
#8290=DIRECTION('center_axis',(0.,0.,1.));
#8291=DIRECTION('ref_axis',(1.,0.,0.));
#8292=DIRECTION('',(-1.,0.,0.));
#8293=DIRECTION('',(0.,-1.,0.));
#8294=DIRECTION('',(-1.,0.,0.));
#8295=DIRECTION('center_axis',(0.,0.,1.));
#8296=DIRECTION('ref_axis',(1.,0.,0.));
#8297=DIRECTION('center_axis',(0.,0.,1.));
#8298=DIRECTION('ref_axis',(1.,0.,0.));
#8299=DIRECTION('center_axis',(0.,0.,1.));
#8300=DIRECTION('ref_axis',(1.,0.,0.));
#8301=DIRECTION('center_axis',(0.,0.,1.));
#8302=DIRECTION('ref_axis',(1.,0.,0.));
#8303=DIRECTION('center_axis',(0.,0.,1.));
#8304=DIRECTION('ref_axis',(1.,0.,0.));
#8305=DIRECTION('',(0.,0.,1.));
#8306=DIRECTION('center_axis',(-1.,0.,0.));
#8307=DIRECTION('ref_axis',(0.,-1.,0.));
#8308=DIRECTION('center_axis',(0.,0.,1.));
#8309=DIRECTION('ref_axis',(1.,0.,0.));
#8310=DIRECTION('',(0.,0.,-1.));
#8311=DIRECTION('center_axis',(0.,1.,0.));
#8312=DIRECTION('ref_axis',(-1.,0.,0.));
#8313=DIRECTION('',(0.,0.,1.));
#8314=DIRECTION('center_axis',(0.,-1.,0.));
#8315=DIRECTION('ref_axis',(1.,0.,0.));
#8316=DIRECTION('',(0.,0.,1.));
#8317=DIRECTION('center_axis',(-1.,0.,0.));
#8318=DIRECTION('ref_axis',(0.,-1.,0.));
#8319=DIRECTION('',(0.,0.,-1.));
#8320=DIRECTION('center_axis',(-1.,0.,0.));
#8321=DIRECTION('ref_axis',(0.,-1.,0.));
#8322=DIRECTION('',(0.,0.,1.));
#8323=DIRECTION('center_axis',(0.,0.,1.));
#8324=DIRECTION('ref_axis',(1.,0.,0.));
#8325=DIRECTION('center_axis',(0.,0.,1.));
#8326=DIRECTION('ref_axis',(1.,0.,0.));
#8327=DIRECTION('center_axis',(0.,0.,1.));
#8328=DIRECTION('ref_axis',(-1.,1.22464679914735E-16,0.));
#8329=DIRECTION('',(0.,0.,1.));
#8330=DIRECTION('',(0.,0.,1.));
#8331=DIRECTION('center_axis',(0.,1.,0.));
#8332=DIRECTION('ref_axis',(-1.,0.,0.));
#8333=DIRECTION('center_axis',(0.,-1.,0.));
#8334=DIRECTION('ref_axis',(1.,0.,0.));
#8335=DIRECTION('center_axis',(0.,0.,1.));
#8336=DIRECTION('ref_axis',(1.,0.,0.));
#8337=DIRECTION('center_axis',(0.,0.,-1.));
#8338=DIRECTION('ref_axis',(1.,0.,0.));
#8339=DIRECTION('center_axis',(0.,0.,1.));
#8340=DIRECTION('ref_axis',(1.,0.,0.));
#8341=DIRECTION('',(0.,0.,-1.));
#8342=DIRECTION('center_axis',(0.,0.,1.));
#8343=DIRECTION('ref_axis',(1.,0.,0.));
#8344=DIRECTION('center_axis',(0.,0.,1.));
#8345=DIRECTION('ref_axis',(1.,0.,0.));
#8346=DIRECTION('axis',(0.,0.,1.));
#8347=DIRECTION('refdir',(1.,0.,0.));
#8348=DIRECTION('center_axis',(0.,0.,1.));
#8349=DIRECTION('ref_axis',(1.,0.,0.));
#8350=DIRECTION('center_axis',(0.,0.,-1.));
#8351=DIRECTION('ref_axis',(1.,0.,0.));
#8352=DIRECTION('',(0.,0.,-1.));
#8353=DIRECTION('center_axis',(0.,0.,-1.));
#8354=DIRECTION('ref_axis',(1.,0.,0.));
#8355=DIRECTION('center_axis',(0.,0.,1.));
#8356=DIRECTION('ref_axis',(1.,0.,0.));
#8357=DIRECTION('center_axis',(0.,0.,1.));
#8358=DIRECTION('ref_axis',(1.,0.,0.));
#8359=DIRECTION('',(0.,0.,-1.));
#8360=DIRECTION('center_axis',(0.,0.,1.));
#8361=DIRECTION('ref_axis',(1.,0.,0.));
#8362=DIRECTION('center_axis',(0.,0.,1.));
#8363=DIRECTION('ref_axis',(1.,0.,0.));
#8364=DIRECTION('center_axis',(0.,0.,1.));
#8365=DIRECTION('ref_axis',(1.,0.,0.));
#8366=DIRECTION('axis',(0.,0.,1.));
#8367=DIRECTION('refdir',(1.,0.,0.));
#8368=DIRECTION('center_axis',(0.,1.,0.));
#8369=DIRECTION('ref_axis',(1.,0.,0.));
#8370=DIRECTION('',(0.,0.,-1.));
#8371=DIRECTION('center_axis',(0.,1.,0.));
#8372=DIRECTION('ref_axis',(1.,0.,0.));
#8373=DIRECTION('center_axis',(0.,1.,0.));
#8374=DIRECTION('ref_axis',(1.,0.,0.));
#8375=DIRECTION('center_axis',(0.,1.,0.));
#8376=DIRECTION('ref_axis',(1.,0.,0.));
#8377=DIRECTION('',(0.,1.,0.));
#8378=DIRECTION('center_axis',(0.,1.,0.));
#8379=DIRECTION('ref_axis',(1.,0.,0.));
#8380=DIRECTION('center_axis',(0.,1.,0.));
#8381=DIRECTION('ref_axis',(1.,0.,0.));
#8382=DIRECTION('',(0.,0.,1.));
#8383=DIRECTION('center_axis',(1.,0.,0.));
#8384=DIRECTION('ref_axis',(0.,0.,-1.));
#8385=DIRECTION('',(0.,0.,-1.));
#8386=DIRECTION('center_axis',(1.,0.,0.));
#8387=DIRECTION('ref_axis',(0.,0.,-1.));
#8388=DIRECTION('center_axis',(1.,0.,0.));
#8389=DIRECTION('ref_axis',(0.,0.,-1.));
#8390=DIRECTION('',(1.,0.,0.));
#8391=DIRECTION('center_axis',(1.,0.,0.));
#8392=DIRECTION('ref_axis',(0.,0.,-1.));
#8393=DIRECTION('center_axis',(1.,0.,0.));
#8394=DIRECTION('ref_axis',(0.,0.,-1.));
#8395=DIRECTION('',(0.,0.,1.));
#8396=DIRECTION('center_axis',(0.,0.,1.));
#8397=DIRECTION('ref_axis',(1.,0.,0.));
#8398=DIRECTION('center_axis',(0.,0.,-1.));
#8399=DIRECTION('ref_axis',(1.,0.,0.));
#8400=DIRECTION('',(0.,0.,-1.));
#8401=DIRECTION('',(0.,0.,-1.));
#8402=DIRECTION('center_axis',(0.,0.,-1.));
#8403=DIRECTION('ref_axis',(1.,0.,0.));
#8404=DIRECTION('center_axis',(0.,0.,1.));
#8405=DIRECTION('ref_axis',(1.,0.,0.));
#8406=DIRECTION('center_axis',(0.,0.,1.));
#8407=DIRECTION('ref_axis',(1.,0.,0.));
#8408=DIRECTION('',(0.,0.,-1.));
#8409=DIRECTION('',(0.,0.,-1.));
#8410=DIRECTION('center_axis',(0.,0.,1.));
#8411=DIRECTION('ref_axis',(1.,0.,0.));
#8412=DIRECTION('center_axis',(0.,0.,1.));
#8413=DIRECTION('ref_axis',(1.,0.,0.));
#8414=DIRECTION('center_axis',(0.,0.,1.));
#8415=DIRECTION('ref_axis',(1.,0.,0.));
#8416=DIRECTION('axis',(0.,0.,1.));
#8417=DIRECTION('refdir',(1.,0.,0.));
#8418=DIRECTION('center_axis',(0.,1.,0.));
#8419=DIRECTION('ref_axis',(1.,0.,0.));
#8420=DIRECTION('center_axis',(0.,1.,0.));
#8421=DIRECTION('ref_axis',(1.,0.,0.));
#8422=DIRECTION('center_axis',(0.866025403784439,0.,-0.5));
#8423=DIRECTION('ref_axis',(0.5,0.,0.866025403784439));
#8424=DIRECTION('',(0.5,0.,0.866025403784439));
#8425=DIRECTION('',(0.,-1.,0.));
#8426=DIRECTION('',(0.5,0.,0.866025403784439));
#8427=DIRECTION('',(0.,-1.,0.));
#8428=DIRECTION('center_axis',(1.20185167898973E-16,0.,-1.));
#8429=DIRECTION('ref_axis',(1.,0.,1.20185167898973E-16));
#8430=DIRECTION('',(1.,0.,1.20185167898973E-16));
#8431=DIRECTION('',(0.,-1.,0.));
#8432=DIRECTION('',(1.,0.,1.20185167898973E-16));
#8433=DIRECTION('center_axis',(-0.866025403784439,0.,-0.5));
#8434=DIRECTION('ref_axis',(0.5,0.,-0.866025403784439));
#8435=DIRECTION('',(0.5,0.,-0.866025403784439));
#8436=DIRECTION('',(0.,-1.,0.));
#8437=DIRECTION('',(0.5,0.,-0.866025403784439));
#8438=DIRECTION('center_axis',(-0.866025403784439,0.,0.5));
#8439=DIRECTION('ref_axis',(-0.5,0.,-0.866025403784439));
#8440=DIRECTION('',(-0.5,0.,-0.866025403784439));
#8441=DIRECTION('',(0.,-1.,0.));
#8442=DIRECTION('',(-0.5,0.,-0.866025403784439));
#8443=DIRECTION('center_axis',(-2.40370335797945E-16,0.,1.));
#8444=DIRECTION('ref_axis',(-1.,0.,-2.40370335797945E-16));
#8445=DIRECTION('',(-1.,0.,-2.40370335797945E-16));
#8446=DIRECTION('',(0.,-1.,0.));
#8447=DIRECTION('',(-1.,0.,-2.40370335797945E-16));
#8448=DIRECTION('center_axis',(0.866025403784439,0.,0.5));
#8449=DIRECTION('ref_axis',(-0.5,0.,0.866025403784439));
#8450=DIRECTION('',(-0.5,0.,0.866025403784439));
#8451=DIRECTION('',(-0.5,0.,0.866025403784439));
#8452=DIRECTION('center_axis',(0.,-1.,0.));
#8453=DIRECTION('ref_axis',(0.,0.,-1.));
#8454=DIRECTION('center_axis',(0.,1.,0.));
#8455=DIRECTION('ref_axis',(0.,0.,1.));
#8456=DIRECTION('center_axis',(0.,-1.,0.));
#8457=DIRECTION('ref_axis',(1.,0.,0.));
#8458=DIRECTION('center_axis',(0.,-1.,0.));
#8459=DIRECTION('ref_axis',(1.,0.,0.));
#8460=DIRECTION('center_axis',(0.,-1.,0.));
#8461=DIRECTION('ref_axis',(1.,0.,0.));
#8462=DIRECTION('',(0.707106781186548,0.707106781186547,8.65956056235494E-17));
#8463=DIRECTION('center_axis',(0.,-1.,0.));
#8464=DIRECTION('ref_axis',(1.,0.,0.));
#8465=DIRECTION('',(0.,1.,0.));
#8466=DIRECTION('',(0.,0.,1.));
#8467=DIRECTION('',(1.,0.,0.));
#8468=DIRECTION('',(0.,0.,1.));
#8469=DIRECTION('',(1.,0.,0.));
#8470=DIRECTION('',(0.,0.,1.));
#8471=DIRECTION('',(1.,0.,0.));
#8472=DIRECTION('',(0.,0.,1.));
#8473=DIRECTION('',(1.,0.,0.));
#8474=DIRECTION('',(0.,0.,1.));
#8475=DIRECTION('',(1.,0.,0.));
#8476=DIRECTION('',(0.,0.,1.));
#8477=DIRECTION('',(1.,0.,0.));
#8478=DIRECTION('',(0.,0.,1.));
#8479=DIRECTION('',(1.,0.,0.));
#8480=DIRECTION('',(0.,0.,1.));
#8481=DIRECTION('',(1.,0.,0.));
#8482=DIRECTION('',(0.,0.,1.));
#8483=DIRECTION('',(-1.,1.22464679914735E-16,0.));
#8484=DIRECTION('',(0.,-1.,2.22044604925031E-16));
#8485=DIRECTION('',(1.,0.,0.));
#8486=DIRECTION('',(0.,0.,1.));
#8487=DIRECTION('',(1.,0.,0.));
#8488=DIRECTION('',(0.,0.,1.));
#8489=DIRECTION('',(1.,0.,0.));
#8490=DIRECTION('',(0.,0.,1.));
#8491=DIRECTION('',(1.,0.,0.));
#8492=DIRECTION('',(0.,0.,1.));
#8493=DIRECTION('',(-1.,1.22464679914735E-16,0.));
#8494=DIRECTION('',(0.,0.,1.));
#8495=DIRECTION('',(1.,0.,0.));
#8496=DIRECTION('',(0.,0.,1.));
#8497=DIRECTION('',(0.999695886388466,-0.024660388034028,0.));
#8498=DIRECTION('',(0.,0.,1.));
#8499=DIRECTION('',(0.998333195372726,0.0577133521542664,0.));
#8500=CARTESIAN_POINT('',(0.,0.,0.));
#8501=CARTESIAN_POINT('',(0.,0.,0.));
#8502=CARTESIAN_POINT('',(0.,0.,0.));
#8503=CARTESIAN_POINT('Origin',(2.52264068711929,2.10639249453345E-16,2.9));
#8504=CARTESIAN_POINT('',(2.35764068711929,1.90432577267413E-16,2.9));
#8505=CARTESIAN_POINT('Origin',(2.52264068711929,2.10639249453345E-16,2.9));
#8506=CARTESIAN_POINT('',(2.35764068711929,2.30845921639276E-16,3.6));
#8507=CARTESIAN_POINT('',(2.35764068711929,1.90432577267413E-16,2.9));
#8508=CARTESIAN_POINT('Origin',(2.52264068711929,2.10639249453345E-16,3.6));
#8509=CARTESIAN_POINT('Origin',(2.52264068711929,2.22044604925031E-16,2.9));
#8510=CARTESIAN_POINT('Origin',(4.24264068711929,1.72,2.9));
#8511=CARTESIAN_POINT('',(4.07764068711929,1.72,2.9));
#8512=CARTESIAN_POINT('Origin',(4.24264068711929,1.72,2.9));
#8513=CARTESIAN_POINT('',(4.07764068711929,1.72,3.6));
#8514=CARTESIAN_POINT('',(4.07764068711929,1.72,2.9));
#8515=CARTESIAN_POINT('Origin',(4.24264068711929,1.72,3.6));
#8516=CARTESIAN_POINT('Origin',(4.24264068711929,1.72,2.9));
#8517=CARTESIAN_POINT('Origin',(5.96264068711929,0.,2.9));
#8518=CARTESIAN_POINT('',(5.79764068711929,-2.02066721859313E-17,2.9));
#8519=CARTESIAN_POINT('Origin',(5.96264068711929,0.,2.9));
#8520=CARTESIAN_POINT('',(5.79764068711929,2.02066721859313E-17,3.6));
#8521=CARTESIAN_POINT('',(5.79764068711929,-2.02066721859313E-17,2.9));
#8522=CARTESIAN_POINT('Origin',(5.96264068711929,0.,3.6));
#8523=CARTESIAN_POINT('Origin',(5.96264068711929,0.,2.9));
#8524=CARTESIAN_POINT('Origin',(4.24264068711929,-1.72,2.9));
#8525=CARTESIAN_POINT('',(4.07764068711929,-1.72,2.9));
#8526=CARTESIAN_POINT('Origin',(4.24264068711929,-1.72,2.9));
#8527=CARTESIAN_POINT('',(4.07764068711929,-1.72,3.6));
#8528=CARTESIAN_POINT('',(4.07764068711929,-1.72,2.9));
#8529=CARTESIAN_POINT('Origin',(4.24264068711929,-1.72,3.6));
#8530=CARTESIAN_POINT('Origin',(4.24264068711929,-1.72,2.9));
#8531=CARTESIAN_POINT('Origin',(4.24264068711929,0.,2.05));
#8532=CARTESIAN_POINT('',(2.74264068711929,-1.83697019872103E-16,2.05));
#8533=CARTESIAN_POINT('Origin',(4.24264068711929,0.,2.05));
#8534=CARTESIAN_POINT('',(2.74264068711929,1.83697019872103E-16,3.6));
#8535=CARTESIAN_POINT('',(2.74264068711929,-1.83697019872103E-16,2.05));
#8536=CARTESIAN_POINT('Origin',(4.24264068711929,0.,3.6));
#8537=CARTESIAN_POINT('Origin',(4.24264068711929,0.,2.05));
#8538=CARTESIAN_POINT('',(3.22264068711929,-1.2491397351303E-16,2.05));
#8539=CARTESIAN_POINT('Origin',(4.24264068711929,0.,2.05));
#8540=CARTESIAN_POINT('Origin',(4.24264068711929,0.,0.9));
#8541=CARTESIAN_POINT('',(3.22264068711929,-1.2491397351303E-16,1.));
#8542=CARTESIAN_POINT('Origin',(4.24264068711929,0.,1.));
#8543=CARTESIAN_POINT('',(3.22264068711929,-1.2491397351303E-16,0.9));
#8544=CARTESIAN_POINT('',(3.99264068711929,-0.988888264668966,1.4));
#8545=CARTESIAN_POINT('Ctrl Pts',(3.99264068711929,-0.988888264668966,1.4));
#8546=CARTESIAN_POINT('Ctrl Pts',(3.99264068711929,-0.988888264668966,1.36846860584118));
#8547=CARTESIAN_POINT('Ctrl Pts',(3.99896863868788,-0.990553370646674,1.33492785033683));
#8548=CARTESIAN_POINT('Ctrl Pts',(4.02452085710491,-0.996491737296663,1.27337379025046));
#8549=CARTESIAN_POINT('Ctrl Pts',(4.04373855891321,-1.00067109353237,1.2453487376128));
#8550=CARTESIAN_POINT('Ctrl Pts',(4.08798657355057,-1.00845756932386,1.20110072297544));
#8551=CARTESIAN_POINT('Ctrl Pts',(4.11601281617403,-1.01258144235289,1.18188079690607));
#8552=CARTESIAN_POINT('Ctrl Pts',(4.17757108672792,-1.0183917429657,1.15632695599232));
#8553=CARTESIAN_POINT('Ctrl Pts',(4.21111335623591,-1.02,1.15));
#8554=CARTESIAN_POINT('Ctrl Pts',(4.27416801800266,-1.02,1.15));
#8555=CARTESIAN_POINT('Ctrl Pts',(4.30771028751065,-1.0183917429657,1.15632695599232));
#8556=CARTESIAN_POINT('Ctrl Pts',(4.36926855806454,-1.01258144235289,1.18188079690607));
#8557=CARTESIAN_POINT('Ctrl Pts',(4.397294800688,-1.00845756932386,1.20110072297544));
#8558=CARTESIAN_POINT('Ctrl Pts',(4.44154281532536,-1.00067109353237,1.2453487376128));
#8559=CARTESIAN_POINT('Ctrl Pts',(4.46076051713366,-0.996491737296663,1.27337379025046));
#8560=CARTESIAN_POINT('Ctrl Pts',(4.48631273555069,-0.990553370646674,1.33492785033683));
#8561=CARTESIAN_POINT('Ctrl Pts',(4.49264068711929,-0.988888264668966,1.36846860584118));
#8562=CARTESIAN_POINT('Ctrl Pts',(4.49264068711929,-0.988888264668966,1.43153139415882));
#8563=CARTESIAN_POINT('Ctrl Pts',(4.48631273555069,-0.990553370646674,1.46507214966317));
#8564=CARTESIAN_POINT('Ctrl Pts',(4.46076051713366,-0.996491737296663,1.52662620974954));
#8565=CARTESIAN_POINT('Ctrl Pts',(4.44154281532536,-1.00067109353237,1.5546512623872));
#8566=CARTESIAN_POINT('Ctrl Pts',(4.397294800688,-1.00845756932386,1.59889927702456));
#8567=CARTESIAN_POINT('Ctrl Pts',(4.36926855806454,-1.01258144235289,1.61811920309393));
#8568=CARTESIAN_POINT('Ctrl Pts',(4.30771028751065,-1.0183917429657,1.64367304400768));
#8569=CARTESIAN_POINT('Ctrl Pts',(4.27416801800266,-1.02,1.65));
#8570=CARTESIAN_POINT('Ctrl Pts',(4.21111335623591,-1.02,1.65));
#8571=CARTESIAN_POINT('Ctrl Pts',(4.17757108672792,-1.0183917429657,1.64367304400768));
#8572=CARTESIAN_POINT('Ctrl Pts',(4.11601281617403,-1.01258144235289,1.61811920309393));
#8573=CARTESIAN_POINT('Ctrl Pts',(4.08798657355057,-1.00845756932386,1.59889927702456));
#8574=CARTESIAN_POINT('Ctrl Pts',(4.04373855891321,-1.00067109353237,1.5546512623872));
#8575=CARTESIAN_POINT('Ctrl Pts',(4.02452085710491,-0.996491737296663,1.52662620974954));
#8576=CARTESIAN_POINT('Ctrl Pts',(3.99896863868788,-0.990553370646674,1.46507214966317));
#8577=CARTESIAN_POINT('Ctrl Pts',(3.99264068711929,-0.988888264668966,1.43153139415882));
#8578=CARTESIAN_POINT('Ctrl Pts',(3.99264068711929,-0.988888264668966,1.4));
#8579=CARTESIAN_POINT('Origin',(-1.72,2.10639249453345E-16,2.9));
#8580=CARTESIAN_POINT('',(-1.885,1.90432577267413E-16,2.9));
#8581=CARTESIAN_POINT('Origin',(-1.72,2.10639249453345E-16,2.9));
#8582=CARTESIAN_POINT('',(-1.885,2.30845921639276E-16,3.6));
#8583=CARTESIAN_POINT('',(-1.885,1.90432577267413E-16,2.9));
#8584=CARTESIAN_POINT('Origin',(-1.72,2.10639249453345E-16,3.6));
#8585=CARTESIAN_POINT('Origin',(-1.72,2.22044604925031E-16,2.9));
#8586=CARTESIAN_POINT('Origin',(1.05319624726672E-16,1.72,2.9));
#8587=CARTESIAN_POINT('',(-0.165,1.72,2.9));
#8588=CARTESIAN_POINT('Origin',(1.05319624726672E-16,1.72,2.9));
#8589=CARTESIAN_POINT('',(-0.165,1.72,3.6));
#8590=CARTESIAN_POINT('',(-0.165,1.72,2.9));
#8591=CARTESIAN_POINT('Origin',(1.05319624726672E-16,1.72,3.6));
#8592=CARTESIAN_POINT('Origin',(1.11022302462516E-16,1.72,2.9));
#8593=CARTESIAN_POINT('Origin',(1.72,0.,2.9));
#8594=CARTESIAN_POINT('',(1.555,-2.02066721859313E-17,2.9));
#8595=CARTESIAN_POINT('Origin',(1.72,0.,2.9));
#8596=CARTESIAN_POINT('',(1.555,2.02066721859313E-17,3.6));
#8597=CARTESIAN_POINT('',(1.555,-2.02066721859313E-17,2.9));
#8598=CARTESIAN_POINT('Origin',(1.72,0.,3.6));
#8599=CARTESIAN_POINT('Origin',(1.72,0.,2.9));
#8600=CARTESIAN_POINT('Origin',(-3.15958874180017E-16,-1.72,2.9));
#8601=CARTESIAN_POINT('',(-0.165,-1.72,2.9));
#8602=CARTESIAN_POINT('Origin',(-3.15958874180017E-16,-1.72,2.9));
#8603=CARTESIAN_POINT('',(-0.165,-1.72,3.6));
#8604=CARTESIAN_POINT('',(-0.165,-1.72,2.9));
#8605=CARTESIAN_POINT('Origin',(-3.15958874180017E-16,-1.72,3.6));
#8606=CARTESIAN_POINT('Origin',(-3.05311331771918E-16,-1.72,2.9));
#8607=CARTESIAN_POINT('Origin',(0.,0.,2.05));
#8608=CARTESIAN_POINT('',(-1.5,-1.83697019872103E-16,2.05));
#8609=CARTESIAN_POINT('Origin',(0.,0.,2.05));
#8610=CARTESIAN_POINT('',(-1.5,1.83697019872103E-16,3.6));
#8611=CARTESIAN_POINT('',(-1.5,-1.83697019872103E-16,2.05));
#8612=CARTESIAN_POINT('Origin',(0.,0.,3.6));
#8613=CARTESIAN_POINT('Origin',(0.,0.,2.05));
#8614=CARTESIAN_POINT('',(-1.02,-1.2491397351303E-16,2.05));
#8615=CARTESIAN_POINT('Origin',(0.,0.,2.05));
#8616=CARTESIAN_POINT('Origin',(0.,0.,0.9));
#8617=CARTESIAN_POINT('',(-1.02,-1.2491397351303E-16,1.));
#8618=CARTESIAN_POINT('Origin',(0.,0.,1.));
#8619=CARTESIAN_POINT('',(-1.02,-1.2491397351303E-16,0.9));
#8620=CARTESIAN_POINT('',(-0.25,-0.988888264668967,1.4));
#8621=CARTESIAN_POINT('Ctrl Pts',(-0.25,-0.988888264668967,1.4));
#8622=CARTESIAN_POINT('Ctrl Pts',(-0.25,-0.988888264668967,1.36846860584118));
#8623=CARTESIAN_POINT('Ctrl Pts',(-0.243672048431404,-0.990553370646674,
1.33492785033683));
#8624=CARTESIAN_POINT('Ctrl Pts',(-0.218119830014375,-0.996491737296663,
1.27337379025046));
#8625=CARTESIAN_POINT('Ctrl Pts',(-0.198902128206072,-1.00067109353237,
1.2453487376128));
#8626=CARTESIAN_POINT('Ctrl Pts',(-0.154654113568716,-1.00845756932386,
1.20110072297544));
#8627=CARTESIAN_POINT('Ctrl Pts',(-0.126627870945253,-1.01258144235289,
1.18188079690607));
#8628=CARTESIAN_POINT('Ctrl Pts',(-0.0650696003913631,-1.0183917429657,
1.15632695599232));
#8629=CARTESIAN_POINT('Ctrl Pts',(-0.031527330883376,-1.02,1.15));
#8630=CARTESIAN_POINT('Ctrl Pts',(0.031527330883376,-1.02,1.15));
#8631=CARTESIAN_POINT('Ctrl Pts',(0.065069600391363,-1.0183917429657,1.15632695599232));
#8632=CARTESIAN_POINT('Ctrl Pts',(0.126627870945253,-1.01258144235289,1.18188079690607));
#8633=CARTESIAN_POINT('Ctrl Pts',(0.154654113568716,-1.00845756932386,1.20110072297544));
#8634=CARTESIAN_POINT('Ctrl Pts',(0.198902128206072,-1.00067109353237,1.2453487376128));
#8635=CARTESIAN_POINT('Ctrl Pts',(0.218119830014375,-0.996491737296663,
1.27337379025046));
#8636=CARTESIAN_POINT('Ctrl Pts',(0.243672048431404,-0.990553370646674,
1.33492785033683));
#8637=CARTESIAN_POINT('Ctrl Pts',(0.25,-0.988888264668967,1.36846860584118));
#8638=CARTESIAN_POINT('Ctrl Pts',(0.25,-0.988888264668967,1.43153139415882));
#8639=CARTESIAN_POINT('Ctrl Pts',(0.243672048431404,-0.990553370646674,
1.46507214966317));
#8640=CARTESIAN_POINT('Ctrl Pts',(0.218119830014375,-0.996491737296663,
1.52662620974954));
#8641=CARTESIAN_POINT('Ctrl Pts',(0.198902128206072,-1.00067109353237,1.5546512623872));
#8642=CARTESIAN_POINT('Ctrl Pts',(0.154654113568716,-1.00845756932386,1.59889927702456));
#8643=CARTESIAN_POINT('Ctrl Pts',(0.126627870945253,-1.01258144235289,1.61811920309393));
#8644=CARTESIAN_POINT('Ctrl Pts',(0.065069600391363,-1.0183917429657,1.64367304400768));
#8645=CARTESIAN_POINT('Ctrl Pts',(0.031527330883376,-1.02,1.65));
#8646=CARTESIAN_POINT('Ctrl Pts',(-0.031527330883376,-1.02,1.65));
#8647=CARTESIAN_POINT('Ctrl Pts',(-0.065069600391363,-1.0183917429657,1.64367304400768));
#8648=CARTESIAN_POINT('Ctrl Pts',(-0.126627870945253,-1.01258144235289,
1.61811920309393));
#8649=CARTESIAN_POINT('Ctrl Pts',(-0.154654113568716,-1.00845756932386,
1.59889927702456));
#8650=CARTESIAN_POINT('Ctrl Pts',(-0.198902128206072,-1.00067109353237,
1.5546512623872));
#8651=CARTESIAN_POINT('Ctrl Pts',(-0.218119830014375,-0.996491737296663,
1.52662620974954));
#8652=CARTESIAN_POINT('Ctrl Pts',(-0.243672048431404,-0.990553370646674,
1.46507214966317));
#8653=CARTESIAN_POINT('Ctrl Pts',(-0.25,-0.988888264668966,1.43153139415882));
#8654=CARTESIAN_POINT('Ctrl Pts',(-0.25,-0.988888264668966,1.4));
#8655=CARTESIAN_POINT('Origin',(5.94264068711928,-1.7,2.2));
#8656=CARTESIAN_POINT('',(5.44264068711928,-1.7,2.2));
#8657=CARTESIAN_POINT('Origin',(5.94264068711928,-1.7,2.2));
#8658=CARTESIAN_POINT('',(5.44264068711928,-1.7,3.6));
#8659=CARTESIAN_POINT('',(5.44264068711928,-1.7,2.2));
#8660=CARTESIAN_POINT('Origin',(5.94264068711928,-1.7,3.6));
#8661=CARTESIAN_POINT('Origin',(5.94264068711928,-1.7,2.2));
#8662=CARTESIAN_POINT('',(5.66764068711928,-1.7,2.2));
#8663=CARTESIAN_POINT('Origin',(5.94264068711928,-1.7,2.2));
#8664=CARTESIAN_POINT('Origin',(-1.7,1.7,2.2));
#8665=CARTESIAN_POINT('',(-2.2,1.7,2.2));
#8666=CARTESIAN_POINT('Origin',(-1.7,1.7,2.2));
#8667=CARTESIAN_POINT('',(-2.2,1.7,3.6));
#8668=CARTESIAN_POINT('',(-2.2,1.7,2.2));
#8669=CARTESIAN_POINT('Origin',(-1.7,1.7,3.6));
#8670=CARTESIAN_POINT('Origin',(-1.7,1.7,2.2));
#8671=CARTESIAN_POINT('',(-1.975,1.7,2.2));
#8672=CARTESIAN_POINT('Origin',(-1.7,1.7,2.2));
#8673=CARTESIAN_POINT('Origin',(-1.7,-1.7,2.2));
#8674=CARTESIAN_POINT('',(-2.2,-1.7,2.2));
#8675=CARTESIAN_POINT('Origin',(-1.7,-1.7,2.2));
#8676=CARTESIAN_POINT('',(-2.2,-1.7,3.6));
#8677=CARTESIAN_POINT('',(-2.2,-1.7,2.2));
#8678=CARTESIAN_POINT('Origin',(-1.7,-1.7,3.6));
#8679=CARTESIAN_POINT('Origin',(-1.7,-1.7,2.2));
#8680=CARTESIAN_POINT('',(-1.975,-1.7,2.2));
#8681=CARTESIAN_POINT('Origin',(-1.7,-1.7,2.2));
#8682=CARTESIAN_POINT('Origin',(5.94264068711928,1.7,2.2));
#8683=CARTESIAN_POINT('',(5.44264068711928,1.7,2.2));
#8684=CARTESIAN_POINT('Origin',(5.94264068711928,1.7,2.2));
#8685=CARTESIAN_POINT('',(5.44264068711928,1.7,3.6));
#8686=CARTESIAN_POINT('',(5.44264068711928,1.7,2.2));
#8687=CARTESIAN_POINT('Origin',(5.94264068711928,1.7,3.6));
#8688=CARTESIAN_POINT('Origin',(5.94264068711928,1.7,2.2));
#8689=CARTESIAN_POINT('',(5.66764068711928,1.7,2.2));
#8690=CARTESIAN_POINT('Origin',(5.94264068711928,1.7,2.2));
#8691=CARTESIAN_POINT('Origin',(5.94264068711928,-1.7,0.9));
#8692=CARTESIAN_POINT('',(5.66764068711928,-1.7,1.));
#8693=CARTESIAN_POINT('Origin',(5.94264068711928,-1.7,1.));
#8694=CARTESIAN_POINT('',(5.66764068711928,-1.7,0.9));
#8695=CARTESIAN_POINT('Origin',(-1.7,1.7,0.9));
#8696=CARTESIAN_POINT('',(-1.975,1.7,1.));
#8697=CARTESIAN_POINT('Origin',(-1.7,1.7,1.));
#8698=CARTESIAN_POINT('',(-1.975,1.7,0.9));
#8699=CARTESIAN_POINT('Origin',(-1.7,-1.7,0.9));
#8700=CARTESIAN_POINT('',(-1.975,-1.7,1.));
#8701=CARTESIAN_POINT('Origin',(-1.7,-1.7,1.));
#8702=CARTESIAN_POINT('',(-1.975,-1.7,0.9));
#8703=CARTESIAN_POINT('Origin',(5.94264068711928,1.7,0.9));
#8704=CARTESIAN_POINT('',(5.66764068711928,1.7,1.));
#8705=CARTESIAN_POINT('Origin',(5.94264068711928,1.7,1.));
#8706=CARTESIAN_POINT('',(5.66764068711928,1.7,0.9));
#8707=CARTESIAN_POINT('Origin',(2.25,0.,1.));
#8708=CARTESIAN_POINT('',(5.73264068711928,1.7,1.));
#8709=CARTESIAN_POINT('Origin',(5.94264068711928,1.7,1.));
#8710=CARTESIAN_POINT('Origin',(2.25,0.,1.));
#8711=CARTESIAN_POINT('',(-1.91,-1.7,1.));
#8712=CARTESIAN_POINT('Origin',(-1.7,-1.7,1.));
#8713=CARTESIAN_POINT('Origin',(2.25,0.,1.));
#8714=CARTESIAN_POINT('',(-1.91,1.7,1.));
#8715=CARTESIAN_POINT('Origin',(-1.7,1.7,1.));
#8716=CARTESIAN_POINT('Origin',(2.25,0.,1.));
#8717=CARTESIAN_POINT('',(5.73264068711928,-1.7,1.));
#8718=CARTESIAN_POINT('Origin',(5.94264068711928,-1.7,1.));
#8719=CARTESIAN_POINT('Origin',(2.25,0.,1.));
#8720=CARTESIAN_POINT('Origin',(2.25,0.,1.));
#8721=CARTESIAN_POINT('Origin',(-2.4,0.,2.3));
#8722=CARTESIAN_POINT('',(-2.4,-2.4,3.6));
#8723=CARTESIAN_POINT('',(-2.4,2.4,3.6));
#8724=CARTESIAN_POINT('',(-2.4,-2.4,3.6));
#8725=CARTESIAN_POINT('',(-2.4,2.4,1.));
#8726=CARTESIAN_POINT('',(-2.4,2.4,3.6));
#8727=CARTESIAN_POINT('',(-2.4,-2.4,1.));
#8728=CARTESIAN_POINT('',(-2.4,0.,1.));
#8729=CARTESIAN_POINT('',(-2.4,-2.4,1.));
#8730=CARTESIAN_POINT('Origin',(2.22132034355964,2.4,2.3));
#8731=CARTESIAN_POINT('',(6.64264068711929,2.4,1.));
#8732=CARTESIAN_POINT('',(0.0249999999999999,2.4,1.));
#8733=CARTESIAN_POINT('',(6.64264068711929,2.4,3.6));
#8734=CARTESIAN_POINT('',(-2.2,2.4,3.6));
#8735=CARTESIAN_POINT('',(6.64264068711929,2.4,3.6));
#8736=CARTESIAN_POINT('Origin',(6.64264068711929,-0.1,2.3));
#8737=CARTESIAN_POINT('',(6.64264068711929,-2.4,1.));
#8738=CARTESIAN_POINT('',(6.64264068711929,1.1,1.));
#8739=CARTESIAN_POINT('',(6.64264068711929,-2.4,3.6));
#8740=CARTESIAN_POINT('',(6.64264068711929,2.2,3.6));
#8741=CARTESIAN_POINT('',(6.64264068711929,-2.4,3.6));
#8742=CARTESIAN_POINT('Origin',(4.24264068711929,-2.2,1.4));
#8743=CARTESIAN_POINT('',(3.99264068711929,-2.4,1.4));
#8744=CARTESIAN_POINT('Origin',(4.24264068711929,-2.4,1.4));
#8745=CARTESIAN_POINT('',(3.99264068711929,-2.2,1.4));
#8746=CARTESIAN_POINT('Origin',(0.,-2.2,1.4));
#8747=CARTESIAN_POINT('',(-0.25,-2.4,1.4));
#8748=CARTESIAN_POINT('Origin',(0.,-2.4,1.4));
#8749=CARTESIAN_POINT('',(-0.25,-2.2,1.4));
#8750=CARTESIAN_POINT('Origin',(6.44264068711929,-2.2,3.6));
#8751=CARTESIAN_POINT('',(6.44264068711928,-2.4,3.6));
#8752=CARTESIAN_POINT('Origin',(2.12132034355964,-2.4,2.3));
#8753=CARTESIAN_POINT('',(0.0249999999999999,-2.4,1.));
#8754=CARTESIAN_POINT('Origin',(9.,-4.3,-0.1));
#8755=CARTESIAN_POINT('',(8.67,-4.3,0.));
#8756=CARTESIAN_POINT('Origin',(9.,-4.3,0.));
#8757=CARTESIAN_POINT('',(8.67,-4.3,1.));
#8758=CARTESIAN_POINT('',(8.67,-4.3,-0.1));
#8759=CARTESIAN_POINT('Origin',(9.,-4.3,1.));
#8760=CARTESIAN_POINT('Origin',(-4.,4.3,-0.1));
#8761=CARTESIAN_POINT('',(-4.33,4.3,0.));
#8762=CARTESIAN_POINT('Origin',(-4.,4.3,0.));
#8763=CARTESIAN_POINT('',(-4.33,4.3,1.));
#8764=CARTESIAN_POINT('',(-4.33,4.3,-0.1));
#8765=CARTESIAN_POINT('Origin',(-4.,4.3,1.));
#8766=CARTESIAN_POINT('Origin',(-4.,-4.3,-0.1));
#8767=CARTESIAN_POINT('',(-4.33,-4.3,0.));
#8768=CARTESIAN_POINT('Origin',(-4.,-4.3,0.));
#8769=CARTESIAN_POINT('',(-4.33,-4.3,1.));
#8770=CARTESIAN_POINT('',(-4.33,-4.3,-0.1));
#8771=CARTESIAN_POINT('Origin',(-4.,-4.3,1.));
#8772=CARTESIAN_POINT('Origin',(9.,4.3,-0.1));
#8773=CARTESIAN_POINT('',(8.67,4.3,0.));
#8774=CARTESIAN_POINT('Origin',(9.,4.3,0.));
#8775=CARTESIAN_POINT('',(8.67,4.3,1.));
#8776=CARTESIAN_POINT('',(8.67,4.3,-0.1));
#8777=CARTESIAN_POINT('Origin',(9.,4.3,1.));
#8778=CARTESIAN_POINT('Origin',(10.,5.,0.));
#8779=CARTESIAN_POINT('',(10.,5.,0.));
#8780=CARTESIAN_POINT('',(-5.,5.,0.));
#8781=CARTESIAN_POINT('',(10.,5.,0.));
#8782=CARTESIAN_POINT('',(-5.,5.,1.));
#8783=CARTESIAN_POINT('',(-5.,5.,0.));
#8784=CARTESIAN_POINT('',(10.,5.,1.));
#8785=CARTESIAN_POINT('',(10.,5.,1.));
#8786=CARTESIAN_POINT('',(10.,5.,0.));
#8787=CARTESIAN_POINT('Origin',(10.,-5.,0.));
#8788=CARTESIAN_POINT('',(10.,-5.,0.));
#8789=CARTESIAN_POINT('',(10.,-5.,0.));
#8790=CARTESIAN_POINT('',(10.,-5.,1.));
#8791=CARTESIAN_POINT('',(10.,-5.,1.));
#8792=CARTESIAN_POINT('',(10.,-5.,0.));
#8793=CARTESIAN_POINT('Origin',(8.,-5.,0.));
#8794=CARTESIAN_POINT('',(-5.,-5.,0.));
#8795=CARTESIAN_POINT('',(-5.,-5.,0.));
#8796=CARTESIAN_POINT('',(-5.,-5.,1.));
#8797=CARTESIAN_POINT('',(-5.,-5.,1.));
#8798=CARTESIAN_POINT('',(-5.,-5.,0.));
#8799=CARTESIAN_POINT('Origin',(-5.,5.,0.));
#8800=CARTESIAN_POINT('',(-5.,5.,0.));
#8801=CARTESIAN_POINT('',(-5.,5.,1.));
#8802=CARTESIAN_POINT('Origin',(5.94264068711928,-1.7,-0.1));
#8803=CARTESIAN_POINT('',(5.73264068711928,-1.7,0.));
#8804=CARTESIAN_POINT('Origin',(5.94264068711928,-1.7,0.));
#8805=CARTESIAN_POINT('',(5.73264068711928,-1.7,-0.1));
#8806=CARTESIAN_POINT('Origin',(-1.7,1.7,-0.1));
#8807=CARTESIAN_POINT('',(-1.91,1.7,0.));
#8808=CARTESIAN_POINT('Origin',(-1.7,1.7,0.));
#8809=CARTESIAN_POINT('',(-1.91,1.7,-0.1));
#8810=CARTESIAN_POINT('Origin',(-1.7,-1.7,-0.1));
#8811=CARTESIAN_POINT('',(-1.91,-1.7,0.));
#8812=CARTESIAN_POINT('Origin',(-1.7,-1.7,0.));
#8813=CARTESIAN_POINT('',(-1.91,-1.7,-0.1));
#8814=CARTESIAN_POINT('Origin',(5.94264068711928,1.7,-0.1));
#8815=CARTESIAN_POINT('',(5.73264068711928,1.7,0.));
#8816=CARTESIAN_POINT('Origin',(5.94264068711928,1.7,0.));
#8817=CARTESIAN_POINT('',(5.73264068711928,1.7,-0.1));
#8818=CARTESIAN_POINT('Origin',(2.25,0.,1.));
#8819=CARTESIAN_POINT('Origin',(2.25,0.,0.));
#8820=CARTESIAN_POINT('',(0.,0.,0.));
#8821=CARTESIAN_POINT('Origin',(8.,-3.2,-0.6));
#8822=CARTESIAN_POINT('',(8.,-3.2,-0.6));
#8823=CARTESIAN_POINT('',(-3.5,-3.2,-0.6));
#8824=CARTESIAN_POINT('',(8.,-3.2,-0.6));
#8825=CARTESIAN_POINT('',(-3.5,-3.2,0.));
#8826=CARTESIAN_POINT('',(-3.5,-3.2,-0.6));
#8827=CARTESIAN_POINT('',(8.,-3.2,0.));
#8828=CARTESIAN_POINT('',(8.,-3.2,0.));
#8829=CARTESIAN_POINT('',(8.,-3.2,-0.6));
#8830=CARTESIAN_POINT('Origin',(8.,-4.,-0.6));
#8831=CARTESIAN_POINT('',(8.,-4.,-0.6));
#8832=CARTESIAN_POINT('',(8.,-4.,-0.6));
#8833=CARTESIAN_POINT('',(8.,-4.,0.));
#8834=CARTESIAN_POINT('',(8.,-4.,0.));
#8835=CARTESIAN_POINT('',(8.,-4.,-0.6));
#8836=CARTESIAN_POINT('Origin',(-3.5,-4.,-0.6));
#8837=CARTESIAN_POINT('',(-3.5,-4.,-0.6));
#8838=CARTESIAN_POINT('',(-3.5,-4.,-0.6));
#8839=CARTESIAN_POINT('',(-3.5,-4.,0.));
#8840=CARTESIAN_POINT('',(-3.5,-4.,0.));
#8841=CARTESIAN_POINT('',(-3.5,-4.,-0.6));
#8842=CARTESIAN_POINT('Origin',(-3.5,-3.2,-0.6));
#8843=CARTESIAN_POINT('',(-3.5,-3.2,-0.6));
#8844=CARTESIAN_POINT('',(-3.5,-3.2,0.));
#8845=CARTESIAN_POINT('Origin',(2.25,-3.6,0.));
#8846=CARTESIAN_POINT('Origin',(2.25,-3.6,-0.6));
#8847=CARTESIAN_POINT('',(0.,0.,0.));
#8848=CARTESIAN_POINT('Origin',(8.,4.,-0.6));
#8849=CARTESIAN_POINT('',(8.,4.,-0.6));
#8850=CARTESIAN_POINT('',(-3.5,4.,-0.6));
#8851=CARTESIAN_POINT('',(8.,4.,-0.6));
#8852=CARTESIAN_POINT('',(-3.5,4.,0.));
#8853=CARTESIAN_POINT('',(-3.5,4.,-0.6));
#8854=CARTESIAN_POINT('',(8.,4.,0.));
#8855=CARTESIAN_POINT('',(8.,4.,0.));
#8856=CARTESIAN_POINT('',(8.,4.,-0.6));
#8857=CARTESIAN_POINT('Origin',(8.,3.2,-0.6));
#8858=CARTESIAN_POINT('',(8.,3.2,-0.6));
#8859=CARTESIAN_POINT('',(8.,3.2,-0.6));
#8860=CARTESIAN_POINT('',(8.,3.2,0.));
#8861=CARTESIAN_POINT('',(8.,3.2,0.));
#8862=CARTESIAN_POINT('',(8.,3.2,-0.6));
#8863=CARTESIAN_POINT('Origin',(-3.5,3.2,-0.6));
#8864=CARTESIAN_POINT('',(-3.5,3.2,-0.6));
#8865=CARTESIAN_POINT('',(-3.5,3.2,-0.6));
#8866=CARTESIAN_POINT('',(-3.5,3.2,0.));
#8867=CARTESIAN_POINT('',(-3.5,3.2,0.));
#8868=CARTESIAN_POINT('',(-3.5,3.2,-0.6));
#8869=CARTESIAN_POINT('Origin',(-3.5,4.,-0.6));
#8870=CARTESIAN_POINT('',(-3.5,4.,-0.6));
#8871=CARTESIAN_POINT('',(-3.5,4.,0.));
#8872=CARTESIAN_POINT('Origin',(2.25,3.6,0.));
#8873=CARTESIAN_POINT('Origin',(2.25,3.6,-0.6));
#8874=CARTESIAN_POINT('',(0.,0.,0.));
#8875=CARTESIAN_POINT('Origin',(-1.72,2.10639249453345E-16,4.));
#8876=CARTESIAN_POINT('',(-1.9819113372093,0.268379305165721,4.));
#8877=CARTESIAN_POINT('',(-1.9819113372093,0.26837930516572,4.4));
#8878=CARTESIAN_POINT('',(-1.9819113372093,0.268379305165721,4.));
#8879=CARTESIAN_POINT('',(-1.9819113372093,-0.268379305165721,4.));
#8880=CARTESIAN_POINT('Origin',(-1.72,2.10639249453345E-16,4.));
#8881=CARTESIAN_POINT('',(-1.9819113372093,-0.268379305165719,4.4));
#8882=CARTESIAN_POINT('',(-1.9819113372093,-0.268379305165721,4.));
#8883=CARTESIAN_POINT('Origin',(-1.72,2.10639249453345E-16,4.4));
#8884=CARTESIAN_POINT('Origin',(-1.72,2.22044604925031E-16,4.));
#8885=CARTESIAN_POINT('',(-2.,-2.44929359829471E-16,4.));
#8886=CARTESIAN_POINT('Origin',(0.,0.,4.));
#8887=CARTESIAN_POINT('Origin',(0.,0.,4.));
#8888=CARTESIAN_POINT('',(-1.945,1.83084696472529E-16,4.));
#8889=CARTESIAN_POINT('Origin',(-1.72,2.10639249453345E-16,4.));
#8890=CARTESIAN_POINT('Origin',(1.11022302462516E-16,1.72,4.));
#8891=CARTESIAN_POINT('',(-0.268379305165721,1.9819113372093,4.));
#8892=CARTESIAN_POINT('',(0.268379305165721,1.9819113372093,4.));
#8893=CARTESIAN_POINT('Origin',(0.,0.,4.));
#8894=CARTESIAN_POINT('Origin',(1.05319624726672E-16,1.72,4.));
#8895=CARTESIAN_POINT('',(-0.225,1.72,4.));
#8896=CARTESIAN_POINT('Origin',(1.05319624726672E-16,1.72,4.));
#8897=CARTESIAN_POINT('Origin',(1.05319624726672E-16,1.72,4.));
#8898=CARTESIAN_POINT('',(-0.26837930516572,1.9819113372093,4.4));
#8899=CARTESIAN_POINT('',(-0.268379305165721,1.9819113372093,4.));
#8900=CARTESIAN_POINT('',(0.26837930516572,1.9819113372093,4.4));
#8901=CARTESIAN_POINT('Origin',(1.05319624726672E-16,1.72,4.4));
#8902=CARTESIAN_POINT('',(0.268379305165721,1.9819113372093,4.));
#8903=CARTESIAN_POINT('Origin',(1.72,0.,4.));
#8904=CARTESIAN_POINT('',(1.9819113372093,0.268379305165721,4.));
#8905=CARTESIAN_POINT('',(1.9819113372093,-0.268379305165721,4.));
#8906=CARTESIAN_POINT('Origin',(0.,0.,4.));
#8907=CARTESIAN_POINT('Origin',(1.72,0.,4.));
#8908=CARTESIAN_POINT('',(1.495,-2.75545529808155E-17,4.));
#8909=CARTESIAN_POINT('Origin',(1.72,0.,4.));
#8910=CARTESIAN_POINT('Origin',(1.72,0.,4.));
#8911=CARTESIAN_POINT('',(1.9819113372093,0.26837930516572,4.4));
#8912=CARTESIAN_POINT('',(1.9819113372093,0.268379305165721,4.));
#8913=CARTESIAN_POINT('',(1.9819113372093,-0.26837930516572,4.4));
#8914=CARTESIAN_POINT('Origin',(1.72,0.,4.4));
#8915=CARTESIAN_POINT('',(1.9819113372093,-0.268379305165721,4.));
#8916=CARTESIAN_POINT('Origin',(-3.33066907387547E-16,-1.72,4.));
#8917=CARTESIAN_POINT('',(0.26837930516572,-1.9819113372093,4.));
#8918=CARTESIAN_POINT('',(-0.268379305165721,-1.9819113372093,4.));
#8919=CARTESIAN_POINT('Origin',(0.,0.,4.));
#8920=CARTESIAN_POINT('Origin',(-3.15958874180017E-16,-1.72,4.));
#8921=CARTESIAN_POINT('',(-0.225,-1.72,4.));
#8922=CARTESIAN_POINT('Origin',(-3.15958874180017E-16,-1.72,4.));
#8923=CARTESIAN_POINT('Origin',(-3.15958874180017E-16,-1.72,4.));
#8924=CARTESIAN_POINT('',(0.268379305165719,-1.9819113372093,4.4));
#8925=CARTESIAN_POINT('',(0.26837930516572,-1.9819113372093,4.));
#8926=CARTESIAN_POINT('',(-0.26837930516572,-1.9819113372093,4.4));
#8927=CARTESIAN_POINT('Origin',(-3.15958874180017E-16,-1.72,4.4));
#8928=CARTESIAN_POINT('',(-0.268379305165721,-1.9819113372093,4.));
#8929=CARTESIAN_POINT('Origin',(0.,0.,4.4));
#8930=CARTESIAN_POINT('Origin',(0.,0.,4.4));
#8931=CARTESIAN_POINT('Origin',(0.,0.,4.4));
#8932=CARTESIAN_POINT('Origin',(0.,0.,4.4));
#8933=CARTESIAN_POINT('Origin',(0.,0.,4.4));
#8934=CARTESIAN_POINT('',(-0.71,-8.69499227394621E-17,4.4));
#8935=CARTESIAN_POINT('Origin',(0.,0.,4.4));
#8936=CARTESIAN_POINT('Origin',(-1.72,2.10639249453345E-16,3.5));
#8937=CARTESIAN_POINT('',(-1.945,1.83084696472529E-16,3.6));
#8938=CARTESIAN_POINT('Origin',(-1.72,2.10639249453345E-16,3.6));
#8939=CARTESIAN_POINT('',(-1.945,1.83084696472529E-16,3.5));
#8940=CARTESIAN_POINT('Origin',(1.05319624726672E-16,1.72,3.5));
#8941=CARTESIAN_POINT('',(-0.225,1.72,3.6));
#8942=CARTESIAN_POINT('Origin',(1.05319624726672E-16,1.72,3.6));
#8943=CARTESIAN_POINT('',(-0.225,1.72,3.5));
#8944=CARTESIAN_POINT('Origin',(1.72,0.,3.5));
#8945=CARTESIAN_POINT('',(1.495,-2.75545529808155E-17,3.6));
#8946=CARTESIAN_POINT('Origin',(1.72,0.,3.6));
#8947=CARTESIAN_POINT('',(1.495,-2.75545529808155E-17,3.5));
#8948=CARTESIAN_POINT('Origin',(-3.15958874180017E-16,-1.72,3.5));
#8949=CARTESIAN_POINT('',(-0.225,-1.72,3.6));
#8950=CARTESIAN_POINT('Origin',(-3.15958874180017E-16,-1.72,3.6));
#8951=CARTESIAN_POINT('',(-0.225,-1.72,3.5));
#8952=CARTESIAN_POINT('Origin',(0.,0.,2.95));
#8953=CARTESIAN_POINT('',(-1.49,-1.82472373072956E-16,3.6));
#8954=CARTESIAN_POINT('Origin',(0.,0.,3.6));
#8955=CARTESIAN_POINT('',(-1.49,-1.82472373072956E-16,2.95));
#8956=CARTESIAN_POINT('',(-1.49,-1.82472373072956E-16,2.95));
#8957=CARTESIAN_POINT('Origin',(0.,0.,2.95));
#8958=CARTESIAN_POINT('Origin',(0.,0.,2.95));
#8959=CARTESIAN_POINT('',(-0.71,-8.69499227394621E-17,2.95));
#8960=CARTESIAN_POINT('Origin',(0.,0.,2.95));
#8961=CARTESIAN_POINT('Origin',(0.,0.,3.6));
#8962=CARTESIAN_POINT('',(-0.71,-8.69499227394621E-17,3.6));
#8963=CARTESIAN_POINT('Origin',(0.,0.,3.6));
#8964=CARTESIAN_POINT('',(-2.,-2.44929359829471E-16,3.6));
#8965=CARTESIAN_POINT('',(-2.,-2.44929359829471E-16,3.6));
#8966=CARTESIAN_POINT('Origin',(0.,0.,3.6));
#8967=CARTESIAN_POINT('Origin',(0.,0.,3.6));
#8968=CARTESIAN_POINT('',(0.,0.,0.));
#8969=CARTESIAN_POINT('Origin',(2.52264068711929,2.10639249453345E-16,4.));
#8970=CARTESIAN_POINT('',(2.26072934990998,0.268379305165721,4.));
#8971=CARTESIAN_POINT('',(2.26072934990998,0.268379305165722,4.4));
#8972=CARTESIAN_POINT('',(2.26072934990998,0.268379305165721,4.));
#8973=CARTESIAN_POINT('',(2.26072934990998,-0.268379305165721,4.));
#8974=CARTESIAN_POINT('Origin',(2.52264068711929,2.10639249453345E-16,4.));
#8975=CARTESIAN_POINT('',(2.26072934990998,-0.268379305165721,4.4));
#8976=CARTESIAN_POINT('',(2.26072934990998,-0.268379305165721,4.));
#8977=CARTESIAN_POINT('Origin',(2.52264068711929,2.10639249453345E-16,4.4));
#8978=CARTESIAN_POINT('Origin',(2.52264068711929,2.22044604925031E-16,4.));
#8979=CARTESIAN_POINT('',(2.24264068711929,-2.44929359829471E-16,4.));
#8980=CARTESIAN_POINT('Origin',(4.24264068711929,0.,4.));
#8981=CARTESIAN_POINT('Origin',(4.24264068711929,0.,4.));
#8982=CARTESIAN_POINT('',(2.29764068711929,1.83084696472529E-16,4.));
#8983=CARTESIAN_POINT('Origin',(2.52264068711929,2.10639249453345E-16,4.));
#8984=CARTESIAN_POINT('Origin',(4.24264068711929,1.72,4.));
#8985=CARTESIAN_POINT('',(3.97426138195357,1.9819113372093,4.));
#8986=CARTESIAN_POINT('',(4.51101999228501,1.9819113372093,4.));
#8987=CARTESIAN_POINT('Origin',(4.24264068711929,0.,4.));
#8988=CARTESIAN_POINT('Origin',(4.24264068711929,1.72,4.));
#8989=CARTESIAN_POINT('',(4.01764068711929,1.72,4.));
#8990=CARTESIAN_POINT('Origin',(4.24264068711929,1.72,4.));
#8991=CARTESIAN_POINT('Origin',(4.24264068711929,1.72,4.));
#8992=CARTESIAN_POINT('',(3.97426138195357,1.9819113372093,4.4));
#8993=CARTESIAN_POINT('',(3.97426138195357,1.9819113372093,4.));
#8994=CARTESIAN_POINT('',(4.51101999228501,1.9819113372093,4.4));
#8995=CARTESIAN_POINT('Origin',(4.24264068711929,1.72,4.4));
#8996=CARTESIAN_POINT('',(4.51101999228501,1.9819113372093,4.));
#8997=CARTESIAN_POINT('Origin',(5.96264068711929,0.,4.));
#8998=CARTESIAN_POINT('',(6.22455202432859,0.268379305165721,4.));
#8999=CARTESIAN_POINT('',(6.22455202432859,-0.268379305165721,4.));
#9000=CARTESIAN_POINT('Origin',(4.24264068711929,0.,4.));
#9001=CARTESIAN_POINT('Origin',(5.96264068711929,0.,4.));
#9002=CARTESIAN_POINT('',(5.73764068711929,-2.75545529808154E-17,4.));
#9003=CARTESIAN_POINT('Origin',(5.96264068711929,0.,4.));
#9004=CARTESIAN_POINT('Origin',(5.96264068711929,0.,4.));
#9005=CARTESIAN_POINT('',(6.22455202432859,0.26837930516572,4.4));
#9006=CARTESIAN_POINT('',(6.22455202432859,0.268379305165721,4.));
#9007=CARTESIAN_POINT('',(6.22455202432859,-0.26837930516572,4.4));
#9008=CARTESIAN_POINT('Origin',(5.96264068711929,0.,4.4));
#9009=CARTESIAN_POINT('',(6.22455202432859,-0.268379305165721,4.));
#9010=CARTESIAN_POINT('Origin',(4.24264068711929,-1.72,4.));
#9011=CARTESIAN_POINT('',(4.51101999228501,-1.9819113372093,4.));
#9012=CARTESIAN_POINT('',(3.97426138195357,-1.9819113372093,4.));
#9013=CARTESIAN_POINT('Origin',(4.24264068711929,0.,4.));
#9014=CARTESIAN_POINT('Origin',(4.24264068711929,-1.72,4.));
#9015=CARTESIAN_POINT('',(4.01764068711929,-1.72,4.));
#9016=CARTESIAN_POINT('Origin',(4.24264068711929,-1.72,4.));
#9017=CARTESIAN_POINT('Origin',(4.24264068711929,-1.72,4.));
#9018=CARTESIAN_POINT('',(4.51101999228501,-1.9819113372093,4.4));
#9019=CARTESIAN_POINT('',(4.51101999228501,-1.9819113372093,4.));
#9020=CARTESIAN_POINT('',(3.97426138195357,-1.9819113372093,4.4));
#9021=CARTESIAN_POINT('Origin',(4.24264068711929,-1.72,4.4));
#9022=CARTESIAN_POINT('',(3.97426138195357,-1.9819113372093,4.));
#9023=CARTESIAN_POINT('Origin',(4.24264068711929,0.,4.4));
#9024=CARTESIAN_POINT('Origin',(4.24264068711929,0.,4.4));
#9025=CARTESIAN_POINT('Origin',(4.24264068711929,0.,4.4));
#9026=CARTESIAN_POINT('Origin',(4.24264068711929,0.,4.4));
#9027=CARTESIAN_POINT('Origin',(4.24264068711929,0.,4.4));
#9028=CARTESIAN_POINT('',(3.53264068711929,-8.69499227394621E-17,4.4));
#9029=CARTESIAN_POINT('Origin',(4.24264068711929,0.,4.4));
#9030=CARTESIAN_POINT('Origin',(2.52264068711929,2.10639249453345E-16,3.5));
#9031=CARTESIAN_POINT('',(2.29764068711929,1.83084696472529E-16,3.6));
#9032=CARTESIAN_POINT('Origin',(2.52264068711929,2.10639249453345E-16,3.6));
#9033=CARTESIAN_POINT('',(2.29764068711929,1.83084696472529E-16,3.5));
#9034=CARTESIAN_POINT('Origin',(4.24264068711929,1.72,3.5));
#9035=CARTESIAN_POINT('',(4.01764068711929,1.72,3.6));
#9036=CARTESIAN_POINT('Origin',(4.24264068711929,1.72,3.6));
#9037=CARTESIAN_POINT('',(4.01764068711929,1.72,3.5));
#9038=CARTESIAN_POINT('Origin',(5.96264068711929,0.,3.5));
#9039=CARTESIAN_POINT('',(5.73764068711929,-2.75545529808154E-17,3.6));
#9040=CARTESIAN_POINT('Origin',(5.96264068711929,0.,3.6));
#9041=CARTESIAN_POINT('',(5.73764068711929,-2.75545529808154E-17,3.5));
#9042=CARTESIAN_POINT('Origin',(4.24264068711929,-1.72,3.5));
#9043=CARTESIAN_POINT('',(4.01764068711929,-1.72,3.6));
#9044=CARTESIAN_POINT('Origin',(4.24264068711929,-1.72,3.6));
#9045=CARTESIAN_POINT('',(4.01764068711929,-1.72,3.5));
#9046=CARTESIAN_POINT('Origin',(4.24264068711929,0.,2.95));
#9047=CARTESIAN_POINT('',(2.75264068711929,-1.82472373072956E-16,3.6));
#9048=CARTESIAN_POINT('Origin',(4.24264068711929,0.,3.6));
#9049=CARTESIAN_POINT('',(2.75264068711929,-1.82472373072956E-16,2.95));
#9050=CARTESIAN_POINT('',(2.75264068711929,-1.82472373072956E-16,2.95));
#9051=CARTESIAN_POINT('Origin',(4.24264068711929,0.,2.95));
#9052=CARTESIAN_POINT('Origin',(4.24264068711929,0.,2.95));
#9053=CARTESIAN_POINT('',(3.53264068711929,-8.69499227394621E-17,2.95));
#9054=CARTESIAN_POINT('Origin',(4.24264068711929,0.,2.95));
#9055=CARTESIAN_POINT('Origin',(4.24264068711929,0.,3.6));
#9056=CARTESIAN_POINT('',(3.53264068711929,-8.69499227394621E-17,3.6));
#9057=CARTESIAN_POINT('Origin',(4.24264068711929,0.,3.6));
#9058=CARTESIAN_POINT('',(2.24264068711929,-2.44929359829471E-16,3.6));
#9059=CARTESIAN_POINT('',(2.24264068711929,-2.44929359829471E-16,3.6));
#9060=CARTESIAN_POINT('Origin',(4.24264068711929,0.,3.6));
#9061=CARTESIAN_POINT('Origin',(4.24264068711929,0.,3.6));
#9062=CARTESIAN_POINT('',(0.,0.,0.));
#9063=CARTESIAN_POINT('Origin',(0.375,0.5,0.));
#9064=CARTESIAN_POINT('',(-0.375,0.5,-4.59242549680257E-17));
#9065=CARTESIAN_POINT('Origin',(0.,0.5,0.));
#9066=CARTESIAN_POINT('Origin',(0.,0.475,0.));
#9067=CARTESIAN_POINT('',(-0.425,0.45,-5.20474889637625E-17));
#9068=CARTESIAN_POINT('Origin',(0.,0.45,0.));
#9069=CARTESIAN_POINT('',(-0.4,0.475,-4.89858719658941E-17));
#9070=CARTESIAN_POINT('Origin',(0.,0.24,0.));
#9071=CARTESIAN_POINT('',(-0.425,0.0299999999999998,-5.20474889637625E-17));
#9072=CARTESIAN_POINT('Origin',(0.,0.0299999999999998,0.));
#9073=CARTESIAN_POINT('',(-0.425,0.24,-5.20474889637625E-17));
#9074=CARTESIAN_POINT('Origin',(0.,0.0150000000000001,0.));
#9075=CARTESIAN_POINT('',(-0.395,4.85722573273506E-17,-4.83735485663204E-17));
#9076=CARTESIAN_POINT('Origin',(0.,0.,0.));
#9077=CARTESIAN_POINT('',(-0.41,0.0150000000000001,-5.02105187650415E-17));
#9078=CARTESIAN_POINT('Origin',(0.27,0.,0.));
#9079=CARTESIAN_POINT('',(-0.27,0.,-3.30654635769785E-17));
#9080=CARTESIAN_POINT('Origin',(0.,0.,0.));
#9081=CARTESIAN_POINT('Origin',(0.,-0.02,0.));
#9082=CARTESIAN_POINT('',(-0.24505,-0.0498999999999999,3.00099698131059E-17));
#9083=CARTESIAN_POINT('Origin',(0.,-0.0498999999999999,0.));
#9084=CARTESIAN_POINT('',(-0.26,-0.02,-3.18408167778312E-17));
#9085=CARTESIAN_POINT('Origin',(0.,-0.995,0.));
#9086=CARTESIAN_POINT('',(-0.24505,-1.95495,3.00099698131059E-17));
#9087=CARTESIAN_POINT('Origin',(0.,-1.95495,0.));
#9088=CARTESIAN_POINT('',(-0.24505,-0.995,-3.00099698131059E-17));
#9089=CARTESIAN_POINT('Origin',(0.,-1.975,0.));
#9090=CARTESIAN_POINT('',(-0.2,-2.,-2.44929359829471E-17));
#9091=CARTESIAN_POINT('Origin',(0.,-2.,0.));
#9092=CARTESIAN_POINT('',(-0.225,-1.975,-2.75545529808154E-17));
#9093=CARTESIAN_POINT('Origin',(0.,-2.,0.));
#9094=CARTESIAN_POINT('Origin',(0.115470053837925,-0.5,-0.2));
#9095=CARTESIAN_POINT('',(0.23094010767585,-0.5,0.));
#9096=CARTESIAN_POINT('',(0.115470053837925,-0.5,-0.2));
#9097=CARTESIAN_POINT('',(0.23094010767585,-0.5,0.));
#9098=CARTESIAN_POINT('',(0.115470053837925,-0.8,-0.2));
#9099=CARTESIAN_POINT('',(0.115470053837925,-0.5,-0.2));
#9100=CARTESIAN_POINT('',(0.23094010767585,-0.8,0.));
#9101=CARTESIAN_POINT('',(0.23094010767585,-0.8,0.));
#9102=CARTESIAN_POINT('',(0.23094010767585,-0.5,0.));
#9103=CARTESIAN_POINT('Origin',(-0.115470053837925,-0.5,-0.2));
#9104=CARTESIAN_POINT('',(-0.115470053837925,-0.5,-0.2));
#9105=CARTESIAN_POINT('',(0.115470053837925,-0.5,-0.2));
#9106=CARTESIAN_POINT('',(-0.115470053837925,-0.8,-0.2));
#9107=CARTESIAN_POINT('',(-0.115470053837925,-0.5,-0.2));
#9108=CARTESIAN_POINT('',(0.115470053837925,-0.8,-0.2));
#9109=CARTESIAN_POINT('Origin',(-0.23094010767585,-0.5,-2.77555756156289E-17));
#9110=CARTESIAN_POINT('',(-0.23094010767585,-0.5,-2.82820063659975E-17));
#9111=CARTESIAN_POINT('',(-0.115470053837925,-0.5,-0.2));
#9112=CARTESIAN_POINT('',(-0.23094010767585,-0.8,-2.77555756156289E-17));
#9113=CARTESIAN_POINT('',(-0.23094010767585,-0.5,-2.82820063659975E-17));
#9114=CARTESIAN_POINT('',(-0.115470053837925,-0.8,-0.2));
#9115=CARTESIAN_POINT('Origin',(-0.115470053837925,-0.5,0.2));
#9116=CARTESIAN_POINT('',(-0.115470053837925,-0.5,0.2));
#9117=CARTESIAN_POINT('',(-0.23094010767585,-0.5,-2.82820063659975E-17));
#9118=CARTESIAN_POINT('',(-0.115470053837925,-0.8,0.2));
#9119=CARTESIAN_POINT('',(-0.115470053837925,-0.5,0.2));
#9120=CARTESIAN_POINT('',(-0.23094010767585,-0.8,-2.82820063659975E-17));
#9121=CARTESIAN_POINT('Origin',(0.115470053837925,-0.5,0.2));
#9122=CARTESIAN_POINT('',(0.115470053837925,-0.5,0.2));
#9123=CARTESIAN_POINT('',(-0.115470053837925,-0.5,0.2));
#9124=CARTESIAN_POINT('',(0.115470053837925,-0.8,0.2));
#9125=CARTESIAN_POINT('',(0.115470053837925,-0.5,0.2));
#9126=CARTESIAN_POINT('',(-0.115470053837925,-0.8,0.2));
#9127=CARTESIAN_POINT('Origin',(0.23094010767585,-0.5,0.));
#9128=CARTESIAN_POINT('',(0.115470053837925,-0.5,0.2));
#9129=CARTESIAN_POINT('',(0.115470053837925,-0.8,0.2));
#9130=CARTESIAN_POINT('Origin',(0.,-0.5,0.));
#9131=CARTESIAN_POINT('Origin',(0.,-0.8,0.));
#9132=CARTESIAN_POINT('',(0.,0.,0.));
#9133=CARTESIAN_POINT('',(0.,0.,0.));
#9134=CARTESIAN_POINT('Origin',(0.,0.,0.));
#9135=CARTESIAN_POINT('',(-0.976185,-0.246528389340863,-1.19548183562566E-16));
#9136=CARTESIAN_POINT('',(-1.19548183562566E-16,-0.246528389340863,0.976185));
#9137=CARTESIAN_POINT('Origin',(0.,-0.246528389340863,0.));
#9138=CARTESIAN_POINT('Origin',(0.,-0.246528389340863,0.));
#9139=CARTESIAN_POINT('',(-1.19548183562566E-16,0.246528389340863,0.976185));
#9140=CARTESIAN_POINT('Origin',(-1.22464679914735E-16,0.,1.));
#9141=CARTESIAN_POINT('',(-0.976185,0.246528389340863,1.19548183562566E-16));
#9142=CARTESIAN_POINT('Origin',(0.,0.246528389340863,0.));
#9143=CARTESIAN_POINT('Origin',(0.,0.246528389340863,0.));
#9144=CARTESIAN_POINT('Origin',(0.,0.,0.));
#9145=CARTESIAN_POINT('',(-0.976185,0.45,-1.19548183562566E-16));
#9146=CARTESIAN_POINT('',(-0.976185,0.,-1.19548183562566E-16));
#9147=CARTESIAN_POINT('Origin',(0.,0.45,0.));
#9148=CARTESIAN_POINT('Origin',(0.,0.,0.));
#9149=CARTESIAN_POINT('',(-0.5,-0.39,-6.12323399573677E-17));
#9150=CARTESIAN_POINT('Origin',(0.,-0.39,0.));
#9151=CARTESIAN_POINT('',(-0.5,0.39,-6.12323399573677E-17));
#9152=CARTESIAN_POINT('',(-0.5,0.,-6.12323399573677E-17));
#9153=CARTESIAN_POINT('Origin',(0.,0.39,0.));
#9154=CARTESIAN_POINT('Origin',(0.,0.42,0.));
#9155=CARTESIAN_POINT('',(-0.56,0.45,-6.85802207522518E-17));
#9156=CARTESIAN_POINT('',(-0.53,0.42,-6.49062803548097E-17));
#9157=CARTESIAN_POINT('Origin',(0.,0.45,0.));
#9158=CARTESIAN_POINT('Origin',(0.976185,0.45,0.));
#9159=CARTESIAN_POINT('Origin',(0.,0.,0.));
#9160=CARTESIAN_POINT('',(-0.976185,-0.45,-1.19548183562566E-16));
#9161=CARTESIAN_POINT('Origin',(0.,-0.45,0.));
#9162=CARTESIAN_POINT('',(-0.976185,0.,-1.19548183562566E-16));
#9163=CARTESIAN_POINT('Origin',(0.56,-0.45,0.));
#9164=CARTESIAN_POINT('',(-0.56,-0.45,-6.85802207522518E-17));
#9165=CARTESIAN_POINT('Origin',(0.,-0.45,0.));
#9166=CARTESIAN_POINT('Origin',(0.,-0.42,0.));
#9167=CARTESIAN_POINT('',(-0.53,-0.42,-6.49062803548097E-17));
#9168=CARTESIAN_POINT('',(0.,0.,0.));
#9169=CARTESIAN_POINT('Origin',(0.,0.,0.));
#9170=CARTESIAN_POINT('',(-1.023815,0.246528389340863,-1.25381176266905E-16));
#9171=CARTESIAN_POINT('',(-1.25381176266905E-16,0.246528389340863,1.023815));
#9172=CARTESIAN_POINT('Origin',(0.,0.246528389340863,0.));
#9173=CARTESIAN_POINT('Origin',(0.,0.246528389340863,0.));
#9174=CARTESIAN_POINT('',(-1.25381176266905E-16,-0.246528389340863,1.023815));
#9175=CARTESIAN_POINT('Origin',(-1.22464679914735E-16,0.,1.));
#9176=CARTESIAN_POINT('',(-1.023815,-0.246528389340863,1.25381176266905E-16));
#9177=CARTESIAN_POINT('Origin',(0.,-0.246528389340863,0.));
#9178=CARTESIAN_POINT('Origin',(0.,-0.246528389340863,0.));
#9179=CARTESIAN_POINT('Origin',(0.,0.,0.));
#9180=CARTESIAN_POINT('',(-1.023815,-0.45,-1.25381176266905E-16));
#9181=CARTESIAN_POINT('Origin',(0.,-0.45,0.));
#9182=CARTESIAN_POINT('',(-1.023815,0.,-1.25381176266905E-16));
#9183=CARTESIAN_POINT('Origin',(1.44,0.45,0.));
#9184=CARTESIAN_POINT('',(-1.44,0.45,-1.76349139077219E-16));
#9185=CARTESIAN_POINT('Origin',(0.,0.45,0.));
#9186=CARTESIAN_POINT('',(-1.023815,0.45,-1.25381176266905E-16));
#9187=CARTESIAN_POINT('Origin',(0.,0.45,0.));
#9188=CARTESIAN_POINT('Origin',(0.,0.42,0.));
#9189=CARTESIAN_POINT('',(-1.5,0.39,-1.83697019872103E-16));
#9190=CARTESIAN_POINT('Origin',(0.,0.39,0.));
#9191=CARTESIAN_POINT('',(-1.47,0.42,-1.80023079474661E-16));
#9192=CARTESIAN_POINT('Origin',(0.,0.,0.));
#9193=CARTESIAN_POINT('',(-1.5,-0.39,-1.83697019872103E-16));
#9194=CARTESIAN_POINT('Origin',(0.,-0.39,0.));
#9195=CARTESIAN_POINT('',(-1.5,0.,-1.83697019872103E-16));
#9196=CARTESIAN_POINT('Origin',(0.,-0.42,0.));
#9197=CARTESIAN_POINT('',(-1.44,-0.45,-1.76349139077219E-16));
#9198=CARTESIAN_POINT('Origin',(0.,-0.45,0.));
#9199=CARTESIAN_POINT('',(-1.47,-0.42,-1.80023079474661E-16));
#9200=CARTESIAN_POINT('Origin',(1.023815,-0.45,0.));
#9201=CARTESIAN_POINT('Origin',(0.,0.,0.));
#9202=CARTESIAN_POINT('',(-1.023815,0.,-1.25381176266905E-16));
#9203=CARTESIAN_POINT('',(0.,0.,0.));
#9204=CARTESIAN_POINT('Origin',(1.,0.,0.));
#9205=CARTESIAN_POINT('',(1.,-1.78583896120461E-33,0.23815));
#9206=CARTESIAN_POINT('',(1.,-1.78583896120461E-33,-0.23815));
#9207=CARTESIAN_POINT('Origin',(1.,0.,0.));
#9208=CARTESIAN_POINT('Origin',(0.707106781186548,0.,-0.707106781186547));
#9209=CARTESIAN_POINT('',(0.875504261126124,-1.78583896120461E-33,-0.538709301246971));
#9210=CARTESIAN_POINT('',(0.538709301246971,-1.78583896120461E-33,-0.875504261126124));
#9211=CARTESIAN_POINT('Origin',(0.707106781186548,0.,-0.707106781186547));
#9212=CARTESIAN_POINT('Origin',(6.12323399573677E-17,0.,-1.));
#9213=CARTESIAN_POINT('',(0.23815,-1.78583896120461E-33,-1.));
#9214=CARTESIAN_POINT('',(-0.23815,-1.78583896120461E-33,-1.));
#9215=CARTESIAN_POINT('Origin',(6.12323399573677E-17,0.,-1.));
#9216=CARTESIAN_POINT('Origin',(-0.707106781186547,0.,-0.707106781186548));
#9217=CARTESIAN_POINT('',(-0.538709301246971,-1.78583896120461E-33,-0.875504261126124));
#9218=CARTESIAN_POINT('',(-0.875504261126124,-1.78583896120461E-33,-0.538709301246971));
#9219=CARTESIAN_POINT('Origin',(-0.707106781186547,0.,-0.707106781186548));
#9220=CARTESIAN_POINT('Origin',(-1.,0.,-1.22464679914735E-16));
#9221=CARTESIAN_POINT('',(-1.,-1.78583896120461E-33,-0.23815));
#9222=CARTESIAN_POINT('',(-1.,-1.78583896120461E-33,0.23815));
#9223=CARTESIAN_POINT('Origin',(-1.,0.,-1.22464679914735E-16));
#9224=CARTESIAN_POINT('Origin',(-0.707106781186548,0.,0.707106781186547));
#9225=CARTESIAN_POINT('',(-0.875504261126124,-7.94881478324376E-33,0.538709301246971));
#9226=CARTESIAN_POINT('',(-0.538709301246971,4.37713686083455E-33,0.875504261126124));
#9227=CARTESIAN_POINT('Origin',(-0.707106781186548,0.,0.707106781186547));
#9228=CARTESIAN_POINT('Origin',(-1.83697019872103E-16,0.,1.));
#9229=CARTESIAN_POINT('',(-0.23815,-1.78583896120461E-33,1.));
#9230=CARTESIAN_POINT('',(0.23815,-1.78583896120461E-33,1.));
#9231=CARTESIAN_POINT('Origin',(-1.83697019872103E-16,0.,1.));
#9232=CARTESIAN_POINT('Origin',(0.707106781186547,0.,0.707106781186548));
#9233=CARTESIAN_POINT('',(0.538709301246971,-4.86732687222419E-33,0.875504261126124));
#9234=CARTESIAN_POINT('',(0.875504261126124,1.29564894981497E-33,0.538709301246971));
#9235=CARTESIAN_POINT('Origin',(0.707106781186547,0.,0.707106781186548));
#9236=CARTESIAN_POINT('',(0.,0.,0.));
#9237=CARTESIAN_POINT('Origin',(0.707106781186547,0.,0.707106781186548));
#9238=CARTESIAN_POINT('',(0.504455939115715,-0.04763,0.841298510752802));
#9239=CARTESIAN_POINT('',(0.841298510752802,-0.04763,0.504455939115715));
#9240=CARTESIAN_POINT('Ctrl Pts',(0.504455939115715,-0.04763,0.841298510752802));
#9241=CARTESIAN_POINT('Ctrl Pts',(0.508899795931835,-0.0740444353928835,
0.838633903678357));
#9242=CARTESIAN_POINT('Ctrl Pts',(0.517157748491652,-0.0999305678883309,
0.833661031856294));
#9243=CARTESIAN_POINT('Ctrl Pts',(0.537715343527944,-0.142345102874864,
0.820511285096538));
#9244=CARTESIAN_POINT('Ctrl Pts',(0.548874290046456,-0.159766064500479,
0.813159949759));
#9245=CARTESIAN_POINT('Ctrl Pts',(0.573915184558107,-0.190326085855194,
0.795684265985089));
#9246=CARTESIAN_POINT('Ctrl Pts',(0.587792702767295,-0.203463743702801,
0.78555112003688));
#9247=CARTESIAN_POINT('Ctrl Pts',(0.615966552324775,-0.224161999508995,
0.763642258217233));
#9248=CARTESIAN_POINT('Ctrl Pts',(0.631684198665438,-0.232861760990032,
0.750785745543687));
#9249=CARTESIAN_POINT('Ctrl Pts',(0.663382628119203,-0.244251601209411,
0.722929908501543));
#9250=CARTESIAN_POINT('Ctrl Pts',(0.679352081686668,-0.246942143572133,
0.707917883896095));
#9251=CARTESIAN_POINT('Ctrl Pts',(0.707917883896095,-0.246942143572133,
0.679352081686668));
#9252=CARTESIAN_POINT('Ctrl Pts',(0.722929908501543,-0.244251601209411,
0.663382628119203));
#9253=CARTESIAN_POINT('Ctrl Pts',(0.750785745543687,-0.232861760990032,
0.631684198665439));
#9254=CARTESIAN_POINT('Ctrl Pts',(0.763642258217232,-0.224161999508995,
0.615966552324775));
#9255=CARTESIAN_POINT('Ctrl Pts',(0.78555112003688,-0.203463743702801,0.587792702767295));
#9256=CARTESIAN_POINT('Ctrl Pts',(0.795684265985088,-0.190326085855194,
0.573915184558108));
#9257=CARTESIAN_POINT('Ctrl Pts',(0.813159949759,-0.15976606450048,0.548874290046456));
#9258=CARTESIAN_POINT('Ctrl Pts',(0.820511285096538,-0.142345102874864,
0.537715343527944));
#9259=CARTESIAN_POINT('Ctrl Pts',(0.833661031856294,-0.099930567888331,
0.517157748491653));
#9260=CARTESIAN_POINT('Ctrl Pts',(0.838633903678357,-0.0740444353928835,
0.508899795931835));
#9261=CARTESIAN_POINT('Ctrl Pts',(0.841298510752801,-0.0476299999999999,
0.504455939115715));
#9262=CARTESIAN_POINT('',(0.528110872004958,-0.04763,0.871530771444223));
#9263=CARTESIAN_POINT('Origin',(0.707106781186547,-0.04763,0.707106781186548));
#9264=CARTESIAN_POINT('',(0.871530771444223,-0.04763,0.528110872004959));
#9265=CARTESIAN_POINT('Ctrl Pts',(0.871530771444223,-0.0476300000000001,
0.528110872004958));
#9266=CARTESIAN_POINT('Ctrl Pts',(0.87014664509073,-0.0609922781173483,
0.530395067942936));
#9267=CARTESIAN_POINT('Ctrl Pts',(0.868149331745851,-0.0742967091364493,
0.533674141594226));
#9268=CARTESIAN_POINT('Ctrl Pts',(0.85981294420286,-0.115492077056649,0.54708917182331));
#9269=CARTESIAN_POINT('Ctrl Pts',(0.850993704737257,-0.141695629206859,
0.560922177770136));
#9270=CARTESIAN_POINT('Ctrl Pts',(0.830754510485543,-0.181890537957859,
0.590422647829571));
#9271=CARTESIAN_POINT('Ctrl Pts',(0.816896541396381,-0.201072148666545,
0.609616703125488));
#9272=CARTESIAN_POINT('Ctrl Pts',(0.792310597819928,-0.223955109275652,
0.641117951819998));
#9273=CARTESIAN_POINT('Ctrl Pts',(0.779109323683612,-0.232742381310829,
0.657208095763053));
#9274=CARTESIAN_POINT('Ctrl Pts',(0.750552691816206,-0.244234834628584,
0.68964083160521));
#9275=CARTESIAN_POINT('Ctrl Pts',(0.735185187071673,-0.246942143572133,
0.705971972091755));
#9276=CARTESIAN_POINT('Ctrl Pts',(0.705971972091754,-0.246942143572133,
0.735185187071673));
#9277=CARTESIAN_POINT('Ctrl Pts',(0.689640831605209,-0.244234834628584,
0.750552691816206));
#9278=CARTESIAN_POINT('Ctrl Pts',(0.657208095763052,-0.232742381310829,
0.779109323683612));
#9279=CARTESIAN_POINT('Ctrl Pts',(0.641117951819998,-0.223955109275652,
0.792310597819928));
#9280=CARTESIAN_POINT('Ctrl Pts',(0.609616703125487,-0.201072148666545,
0.816896541396382));
#9281=CARTESIAN_POINT('Ctrl Pts',(0.590422647829571,-0.181890537957858,
0.830754510485544));
#9282=CARTESIAN_POINT('Ctrl Pts',(0.560922177770135,-0.141695629206858,
0.850993704737257));
#9283=CARTESIAN_POINT('Ctrl Pts',(0.547089171823309,-0.115492077056649,
0.859812944202861));
#9284=CARTESIAN_POINT('Ctrl Pts',(0.533674141594226,-0.0742967091364491,
0.868149331745852));
#9285=CARTESIAN_POINT('Ctrl Pts',(0.530395067942936,-0.0609922781173483,
0.870146645090731));
#9286=CARTESIAN_POINT('Ctrl Pts',(0.528110872004958,-0.0476300000000001,
0.871530771444223));
#9287=CARTESIAN_POINT('Origin',(0.707106781186547,-0.04763,0.707106781186548));
#9288=CARTESIAN_POINT('Origin',(0.,-0.166705,0.));
#9289=CARTESIAN_POINT('',(0.242834539687906,-0.04763,0.989696097314));
#9290=CARTESIAN_POINT('Origin',(0.,-0.04763,0.));
#9291=CARTESIAN_POINT('',(-0.242834539687907,-0.04763,0.989696097314));
#9292=CARTESIAN_POINT('Ctrl Pts',(0.242834539687906,-0.04763,0.989696097314));
#9293=CARTESIAN_POINT('Ctrl Pts',(0.24024064412003,-0.0609922781173483,
0.990332542620729));
#9294=CARTESIAN_POINT('Ctrl Pts',(0.236509675094874,-0.0742967091364492,
0.991238884025248));
#9295=CARTESIAN_POINT('Ctrl Pts',(0.221129100087819,-0.115492077056649,
0.994830026707808));
#9296=CARTESIAN_POINT('Ctrl Pts',(0.205111543747588,-0.141695629206859,
0.998375294985966));
#9297=CARTESIAN_POINT('Ctrl Pts',(0.169940289819232,-0.181890537957859,
1.00492400591205));
#9298=CARTESIAN_POINT('Ctrl Pts',(0.1465689792446,-0.201072148666545,1.00869718865384));
#9299=CARTESIAN_POINT('Ctrl Pts',(0.106909345252087,-0.223955109275652,
1.01358704779679));
#9300=CARTESIAN_POINT('Ctrl Pts',(0.0861971848975941,-0.232742381310829,
1.0156297872271));
#9301=CARTESIAN_POINT('Ctrl Pts',(0.0430711894098822,-0.244234834628584,
1.01837060663223));
#9302=CARTESIAN_POINT('Ctrl Pts',(0.0206568624125605,-0.246942143572133,
1.019052));
#9303=CARTESIAN_POINT('Ctrl Pts',(-0.0206568624125608,-0.246942143572133,
1.019052));
#9304=CARTESIAN_POINT('Ctrl Pts',(-0.0430711894098825,-0.244234834628584,
1.01837060663223));
#9305=CARTESIAN_POINT('Ctrl Pts',(-0.0861971848975943,-0.232742381310829,
1.0156297872271));
#9306=CARTESIAN_POINT('Ctrl Pts',(-0.106909345252088,-0.223955109275652,
1.01358704779679));
#9307=CARTESIAN_POINT('Ctrl Pts',(-0.1465689792446,-0.201072148666545,1.00869718865384));
#9308=CARTESIAN_POINT('Ctrl Pts',(-0.169940289819232,-0.181890537957859,
1.00492400591205));
#9309=CARTESIAN_POINT('Ctrl Pts',(-0.205111543747588,-0.141695629206859,
0.998375294985966));
#9310=CARTESIAN_POINT('Ctrl Pts',(-0.221129100087819,-0.115492077056649,
0.994830026707808));
#9311=CARTESIAN_POINT('Ctrl Pts',(-0.236509675094875,-0.0742967091364493,
0.991238884025248));
#9312=CARTESIAN_POINT('Ctrl Pts',(-0.24024064412003,-0.0609922781173483,
0.990332542620729));
#9313=CARTESIAN_POINT('Ctrl Pts',(-0.242834539687907,-0.04763,0.989696097314));
#9314=CARTESIAN_POINT('',(-0.528110872004959,-0.04763,0.871530771444223));
#9315=CARTESIAN_POINT('Origin',(0.,-0.04763,0.));
#9316=CARTESIAN_POINT('',(-0.871530771444223,-0.04763,0.528110872004958));
#9317=CARTESIAN_POINT('Ctrl Pts',(-0.528110872004958,-0.0476300000000001,
0.871530771444223));
#9318=CARTESIAN_POINT('Ctrl Pts',(-0.530395067942936,-0.0609922781173484,
0.87014664509073));
#9319=CARTESIAN_POINT('Ctrl Pts',(-0.533674141594226,-0.0742967091364493,
0.868149331745851));
#9320=CARTESIAN_POINT('Ctrl Pts',(-0.54708917182331,-0.115492077056649,
0.85981294420286));
#9321=CARTESIAN_POINT('Ctrl Pts',(-0.560922177770136,-0.141695629206859,
0.850993704737257));
#9322=CARTESIAN_POINT('Ctrl Pts',(-0.590422647829571,-0.181890537957859,
0.830754510485543));
#9323=CARTESIAN_POINT('Ctrl Pts',(-0.609616703125488,-0.201072148666545,
0.816896541396381));
#9324=CARTESIAN_POINT('Ctrl Pts',(-0.641117951819998,-0.223955109275652,
0.792310597819928));
#9325=CARTESIAN_POINT('Ctrl Pts',(-0.657208095763053,-0.232742381310829,
0.779109323683611));
#9326=CARTESIAN_POINT('Ctrl Pts',(-0.68964083160521,-0.244234834628584,
0.750552691816205));
#9327=CARTESIAN_POINT('Ctrl Pts',(-0.705971972091755,-0.246942143572133,
0.735185187071673));
#9328=CARTESIAN_POINT('Ctrl Pts',(-0.735185187071673,-0.246942143572133,
0.705971972091754));
#9329=CARTESIAN_POINT('Ctrl Pts',(-0.750552691816206,-0.244234834628584,
0.689640831605209));
#9330=CARTESIAN_POINT('Ctrl Pts',(-0.779109323683612,-0.232742381310829,
0.657208095763052));
#9331=CARTESIAN_POINT('Ctrl Pts',(-0.792310597819928,-0.223955109275652,
0.641117951819998));
#9332=CARTESIAN_POINT('Ctrl Pts',(-0.816896541396382,-0.201072148666545,
0.609616703125487));
#9333=CARTESIAN_POINT('Ctrl Pts',(-0.830754510485544,-0.181890537957858,
0.590422647829571));
#9334=CARTESIAN_POINT('Ctrl Pts',(-0.850993704737257,-0.141695629206858,
0.560922177770135));
#9335=CARTESIAN_POINT('Ctrl Pts',(-0.859812944202861,-0.115492077056649,
0.547089171823309));
#9336=CARTESIAN_POINT('Ctrl Pts',(-0.868149331745852,-0.0742967091364491,
0.533674141594226));
#9337=CARTESIAN_POINT('Ctrl Pts',(-0.870146645090731,-0.0609922781173483,
0.530395067942936));
#9338=CARTESIAN_POINT('Ctrl Pts',(-0.871530771444223,-0.04763,0.528110872004958));
#9339=CARTESIAN_POINT('',(-0.989696097314,-0.04763,0.242834539687906));
#9340=CARTESIAN_POINT('Origin',(0.,-0.04763,0.));
#9341=CARTESIAN_POINT('',(-1.019052,-0.246942143572133,1.248489836334E-16));
#9342=CARTESIAN_POINT('Ctrl Pts',(-0.989696097314,-0.04763,0.242834539687906));
#9343=CARTESIAN_POINT('Ctrl Pts',(-0.990332542620729,-0.0609922781173483,
0.24024064412003));
#9344=CARTESIAN_POINT('Ctrl Pts',(-0.991238884025248,-0.0742967091364492,
0.236509675094874));
#9345=CARTESIAN_POINT('Ctrl Pts',(-0.994830026707808,-0.115492077056649,
0.221129100087819));
#9346=CARTESIAN_POINT('Ctrl Pts',(-0.998375294985966,-0.141695629206859,
0.205111543747588));
#9347=CARTESIAN_POINT('Ctrl Pts',(-1.00492400591205,-0.181890537957859,
0.169940289819232));
#9348=CARTESIAN_POINT('Ctrl Pts',(-1.00869718865384,-0.201072148666545,
0.1465689792446));
#9349=CARTESIAN_POINT('Ctrl Pts',(-1.01358704779679,-0.223955109275652,
0.106909345252088));
#9350=CARTESIAN_POINT('Ctrl Pts',(-1.0156297872271,-0.232742381310829,0.0861971848975944));
#9351=CARTESIAN_POINT('Ctrl Pts',(-1.01837060663223,-0.244234834628584,
0.0430711894098825));
#9352=CARTESIAN_POINT('Ctrl Pts',(-1.019052,-0.246942143572133,0.0206568624125608));
#9353=CARTESIAN_POINT('Ctrl Pts',(-1.019052,-0.246942143572133,1.2490009027033E-16));
#9354=CARTESIAN_POINT('',(-1.019052,-0.28578,1.24797876996471E-16));
#9355=CARTESIAN_POINT('',(-1.019052,-0.166705,1.24797876996471E-16));
#9356=CARTESIAN_POINT('Origin',(0.,-0.28578,0.));
#9357=CARTESIAN_POINT('',(-0.989696097314,-0.04763,-0.242834539687906));
#9358=CARTESIAN_POINT('Ctrl Pts',(-1.019052,-0.246942143572133,1.2490009027033E-16));
#9359=CARTESIAN_POINT('Ctrl Pts',(-1.019052,-0.246942143572133,-0.0206568624125605));
#9360=CARTESIAN_POINT('Ctrl Pts',(-1.01837060663223,-0.244234834628584,
-0.0430711894098822));
#9361=CARTESIAN_POINT('Ctrl Pts',(-1.0156297872271,-0.232742381310829,-0.0861971848975941));
#9362=CARTESIAN_POINT('Ctrl Pts',(-1.01358704779679,-0.223955109275652,
-0.106909345252087));
#9363=CARTESIAN_POINT('Ctrl Pts',(-1.00869718865384,-0.201072148666546,
-0.1465689792446));
#9364=CARTESIAN_POINT('Ctrl Pts',(-1.00492400591205,-0.181890537957859,
-0.169940289819232));
#9365=CARTESIAN_POINT('Ctrl Pts',(-0.998375294985966,-0.141695629206859,
-0.205111543747588));
#9366=CARTESIAN_POINT('Ctrl Pts',(-0.994830026707808,-0.11549207705665,
-0.221129100087819));
#9367=CARTESIAN_POINT('Ctrl Pts',(-0.991238884025248,-0.0742967091364495,
-0.236509675094874));
#9368=CARTESIAN_POINT('Ctrl Pts',(-0.990332542620729,-0.0609922781173484,
-0.24024064412003));
#9369=CARTESIAN_POINT('Ctrl Pts',(-0.989696097314,-0.0476300000000001,-0.242834539687907));
#9370=CARTESIAN_POINT('',(-0.871530771444223,-0.04763,-0.528110872004958));
#9371=CARTESIAN_POINT('Origin',(0.,-0.04763,0.));
#9372=CARTESIAN_POINT('',(-0.528110872004958,-0.04763,-0.871530771444223));
#9373=CARTESIAN_POINT('Ctrl Pts',(-0.871530771444223,-0.0476300000000001,
-0.528110872004958));
#9374=CARTESIAN_POINT('Ctrl Pts',(-0.87014664509073,-0.0609922781173484,
-0.530395067942936));
#9375=CARTESIAN_POINT('Ctrl Pts',(-0.868149331745851,-0.0742967091364494,
-0.533674141594226));
#9376=CARTESIAN_POINT('Ctrl Pts',(-0.85981294420286,-0.115492077056649,
-0.54708917182331));
#9377=CARTESIAN_POINT('Ctrl Pts',(-0.850993704737257,-0.141695629206859,
-0.560922177770136));
#9378=CARTESIAN_POINT('Ctrl Pts',(-0.830754510485543,-0.181890537957859,
-0.590422647829571));
#9379=CARTESIAN_POINT('Ctrl Pts',(-0.816896541396381,-0.201072148666546,
-0.609616703125488));
#9380=CARTESIAN_POINT('Ctrl Pts',(-0.792310597819928,-0.223955109275652,
-0.641117951819999));
#9381=CARTESIAN_POINT('Ctrl Pts',(-0.779109323683611,-0.232742381310829,
-0.657208095763053));
#9382=CARTESIAN_POINT('Ctrl Pts',(-0.750552691816205,-0.244234834628584,
-0.68964083160521));
#9383=CARTESIAN_POINT('Ctrl Pts',(-0.735185187071673,-0.246942143572133,
-0.705971972091755));
#9384=CARTESIAN_POINT('Ctrl Pts',(-0.705971972091754,-0.246942143572133,
-0.735185187071673));
#9385=CARTESIAN_POINT('Ctrl Pts',(-0.68964083160521,-0.244234834628584,
-0.750552691816206));
#9386=CARTESIAN_POINT('Ctrl Pts',(-0.657208095763052,-0.232742381310829,
-0.779109323683612));
#9387=CARTESIAN_POINT('Ctrl Pts',(-0.641117951819998,-0.223955109275652,
-0.792310597819928));
#9388=CARTESIAN_POINT('Ctrl Pts',(-0.609616703125488,-0.201072148666545,
-0.816896541396381));
#9389=CARTESIAN_POINT('Ctrl Pts',(-0.590422647829571,-0.181890537957859,
-0.830754510485543));
#9390=CARTESIAN_POINT('Ctrl Pts',(-0.560922177770136,-0.141695629206859,
-0.850993704737257));
#9391=CARTESIAN_POINT('Ctrl Pts',(-0.54708917182331,-0.115492077056649,
-0.85981294420286));
#9392=CARTESIAN_POINT('Ctrl Pts',(-0.533674141594226,-0.0742967091364494,
-0.868149331745852));
#9393=CARTESIAN_POINT('Ctrl Pts',(-0.530395067942936,-0.0609922781173484,
-0.870146645090731));
#9394=CARTESIAN_POINT('Ctrl Pts',(-0.528110872004958,-0.0476300000000001,
-0.871530771444223));
#9395=CARTESIAN_POINT('',(-0.242834539687906,-0.04763,-0.989696097314));
#9396=CARTESIAN_POINT('Origin',(0.,-0.04763,0.));
#9397=CARTESIAN_POINT('',(0.242834539687906,-0.04763,-0.989696097314));
#9398=CARTESIAN_POINT('Ctrl Pts',(-0.242834539687907,-0.04763,-0.989696097314));
#9399=CARTESIAN_POINT('Ctrl Pts',(-0.24024064412003,-0.0609922781173483,
-0.990332542620729));
#9400=CARTESIAN_POINT('Ctrl Pts',(-0.236509675094874,-0.0742967091364493,
-0.991238884025248));
#9401=CARTESIAN_POINT('Ctrl Pts',(-0.221129100087819,-0.115492077056649,
-0.994830026707808));
#9402=CARTESIAN_POINT('Ctrl Pts',(-0.205111543747588,-0.141695629206859,
-0.998375294985966));
#9403=CARTESIAN_POINT('Ctrl Pts',(-0.169940289819232,-0.181890537957859,
-1.00492400591205));
#9404=CARTESIAN_POINT('Ctrl Pts',(-0.1465689792446,-0.201072148666545,-1.00869718865384));
#9405=CARTESIAN_POINT('Ctrl Pts',(-0.106909345252087,-0.223955109275652,
-1.01358704779679));
#9406=CARTESIAN_POINT('Ctrl Pts',(-0.0861971848975942,-0.232742381310829,
-1.0156297872271));
#9407=CARTESIAN_POINT('Ctrl Pts',(-0.0430711894098823,-0.244234834628584,
-1.01837060663223));
#9408=CARTESIAN_POINT('Ctrl Pts',(-0.0206568624125606,-0.246942143572133,
-1.019052));
#9409=CARTESIAN_POINT('Ctrl Pts',(0.0206568624125607,-0.246942143572133,
-1.019052));
#9410=CARTESIAN_POINT('Ctrl Pts',(0.0430711894098824,-0.244234834628584,
-1.01837060663223));
#9411=CARTESIAN_POINT('Ctrl Pts',(0.0861971848975943,-0.232742381310829,
-1.0156297872271));
#9412=CARTESIAN_POINT('Ctrl Pts',(0.106909345252088,-0.223955109275652,
-1.01358704779679));
#9413=CARTESIAN_POINT('Ctrl Pts',(0.1465689792446,-0.201072148666545,-1.00869718865384));
#9414=CARTESIAN_POINT('Ctrl Pts',(0.169940289819232,-0.181890537957859,
-1.00492400591205));
#9415=CARTESIAN_POINT('Ctrl Pts',(0.205111543747588,-0.141695629206859,
-0.998375294985966));
#9416=CARTESIAN_POINT('Ctrl Pts',(0.221129100087819,-0.115492077056649,
-0.994830026707808));
#9417=CARTESIAN_POINT('Ctrl Pts',(0.236509675094874,-0.0742967091364493,
-0.991238884025248));
#9418=CARTESIAN_POINT('Ctrl Pts',(0.24024064412003,-0.0609922781173484,
-0.990332542620729));
#9419=CARTESIAN_POINT('Ctrl Pts',(0.242834539687907,-0.04763,-0.989696097314));
#9420=CARTESIAN_POINT('',(0.528110872004958,-0.04763,-0.871530771444223));
#9421=CARTESIAN_POINT('Origin',(0.,-0.04763,0.));
#9422=CARTESIAN_POINT('',(0.871530771444223,-0.04763,-0.528110872004958));
#9423=CARTESIAN_POINT('Ctrl Pts',(0.528110872004958,-0.0476300000000001,
-0.871530771444223));
#9424=CARTESIAN_POINT('Ctrl Pts',(0.530395067942936,-0.0609922781173484,
-0.870146645090731));
#9425=CARTESIAN_POINT('Ctrl Pts',(0.533674141594226,-0.0742967091364493,
-0.868149331745851));
#9426=CARTESIAN_POINT('Ctrl Pts',(0.54708917182331,-0.115492077056649,-0.85981294420286));
#9427=CARTESIAN_POINT('Ctrl Pts',(0.560922177770136,-0.141695629206859,
-0.850993704737257));
#9428=CARTESIAN_POINT('Ctrl Pts',(0.590422647829571,-0.181890537957859,
-0.830754510485543));
#9429=CARTESIAN_POINT('Ctrl Pts',(0.609616703125488,-0.201072148666545,
-0.816896541396381));
#9430=CARTESIAN_POINT('Ctrl Pts',(0.641117951819998,-0.223955109275652,
-0.792310597819928));
#9431=CARTESIAN_POINT('Ctrl Pts',(0.657208095763053,-0.232742381310829,
-0.779109323683612));
#9432=CARTESIAN_POINT('Ctrl Pts',(0.68964083160521,-0.244234834628584,-0.750552691816206));
#9433=CARTESIAN_POINT('Ctrl Pts',(0.705971972091755,-0.246942143572133,
-0.735185187071673));
#9434=CARTESIAN_POINT('Ctrl Pts',(0.735185187071673,-0.246942143572133,
-0.705971972091754));
#9435=CARTESIAN_POINT('Ctrl Pts',(0.750552691816206,-0.244234834628584,
-0.68964083160521));
#9436=CARTESIAN_POINT('Ctrl Pts',(0.779109323683612,-0.232742381310829,
-0.657208095763053));
#9437=CARTESIAN_POINT('Ctrl Pts',(0.792310597819928,-0.223955109275652,
-0.641117951819998));
#9438=CARTESIAN_POINT('Ctrl Pts',(0.816896541396381,-0.201072148666545,
-0.609616703125488));
#9439=CARTESIAN_POINT('Ctrl Pts',(0.830754510485543,-0.181890537957859,
-0.590422647829571));
#9440=CARTESIAN_POINT('Ctrl Pts',(0.850993704737257,-0.141695629206859,
-0.560922177770136));
#9441=CARTESIAN_POINT('Ctrl Pts',(0.85981294420286,-0.115492077056649,-0.54708917182331));
#9442=CARTESIAN_POINT('Ctrl Pts',(0.868149331745851,-0.0742967091364493,
-0.533674141594226));
#9443=CARTESIAN_POINT('Ctrl Pts',(0.870146645090731,-0.0609922781173484,
-0.530395067942936));
#9444=CARTESIAN_POINT('Ctrl Pts',(0.871530771444223,-0.0476300000000001,
-0.528110872004958));
#9445=CARTESIAN_POINT('',(0.989696097314,-0.04763,-0.242834539687906));
#9446=CARTESIAN_POINT('Origin',(0.,-0.04763,0.));
#9447=CARTESIAN_POINT('',(0.989696097314,-0.04763,0.242834539687906));
#9448=CARTESIAN_POINT('Ctrl Pts',(0.989696097314,-0.04763,-0.242834539687907));
#9449=CARTESIAN_POINT('Ctrl Pts',(0.990332542620729,-0.0609922781173483,
-0.24024064412003));
#9450=CARTESIAN_POINT('Ctrl Pts',(0.991238884025248,-0.0742967091364493,
-0.236509675094874));
#9451=CARTESIAN_POINT('Ctrl Pts',(0.994830026707808,-0.115492077056649,
-0.221129100087819));
#9452=CARTESIAN_POINT('Ctrl Pts',(0.998375294985966,-0.141695629206859,
-0.205111543747588));
#9453=CARTESIAN_POINT('Ctrl Pts',(1.00492400591205,-0.181890537957859,-0.169940289819232));
#9454=CARTESIAN_POINT('Ctrl Pts',(1.00869718865384,-0.201072148666545,-0.1465689792446));
#9455=CARTESIAN_POINT('Ctrl Pts',(1.01358704779679,-0.223955109275652,-0.106909345252087));
#9456=CARTESIAN_POINT('Ctrl Pts',(1.0156297872271,-0.232742381310829,-0.0861971848975942));
#9457=CARTESIAN_POINT('Ctrl Pts',(1.01837060663223,-0.244234834628584,-0.0430711894098823));
#9458=CARTESIAN_POINT('Ctrl Pts',(1.019052,-0.246942143572133,-0.0206568624125607));
#9459=CARTESIAN_POINT('Ctrl Pts',(1.019052,-0.246942143572133,0.0206568624125607));
#9460=CARTESIAN_POINT('Ctrl Pts',(1.01837060663223,-0.244234834628584,0.0430711894098823));
#9461=CARTESIAN_POINT('Ctrl Pts',(1.0156297872271,-0.232742381310829,0.0861971848975942));
#9462=CARTESIAN_POINT('Ctrl Pts',(1.01358704779679,-0.223955109275652,0.106909345252087));
#9463=CARTESIAN_POINT('Ctrl Pts',(1.00869718865384,-0.201072148666545,0.1465689792446));
#9464=CARTESIAN_POINT('Ctrl Pts',(1.00492400591205,-0.181890537957859,0.169940289819232));
#9465=CARTESIAN_POINT('Ctrl Pts',(0.998375294985966,-0.141695629206859,
0.205111543747588));
#9466=CARTESIAN_POINT('Ctrl Pts',(0.994830026707808,-0.115492077056649,
0.221129100087819));
#9467=CARTESIAN_POINT('Ctrl Pts',(0.991238884025248,-0.0742967091364492,
0.236509675094874));
#9468=CARTESIAN_POINT('Ctrl Pts',(0.990332542620729,-0.0609922781173483,
0.24024064412003));
#9469=CARTESIAN_POINT('Ctrl Pts',(0.989696097314,-0.04763,0.242834539687907));
#9470=CARTESIAN_POINT('Origin',(0.,-0.04763,0.));
#9471=CARTESIAN_POINT('Origin',(0.,-0.04763,0.));
#9472=CARTESIAN_POINT('',(0.238183666596899,-0.04763,0.951592097314));
#9473=CARTESIAN_POINT('Origin',(0.,-0.04763,0.));
#9474=CARTESIAN_POINT('Origin',(-1.94289029309402E-16,-0.04763,1.));
#9475=CARTESIAN_POINT('Origin',(-1.94289029309402E-16,0.,1.));
#9476=CARTESIAN_POINT('',(-0.2381836665969,-0.04763,0.951592097314));
#9477=CARTESIAN_POINT('Ctrl Pts',(-0.238183666596899,-0.0476299999999999,
0.951592097314));
#9478=CARTESIAN_POINT('Ctrl Pts',(-0.233157223576062,-0.0740444353928835,
0.952850216871763));
#9479=CARTESIAN_POINT('Ctrl Pts',(-0.223801617934946,-0.0999305678883309,
0.955173119738174));
#9480=CARTESIAN_POINT('Ctrl Pts',(-0.199966927975188,-0.142345102874864,
0.960411259488514));
#9481=CARTESIAN_POINT('Ctrl Pts',(-0.1868781821531,-0.159766064500479,0.963103647174702));
#9482=CARTESIAN_POINT('Ctrl Pts',(-0.15681442133453,-0.190326085855194,
0.968453058988463));
#9483=CARTESIAN_POINT('Ctrl Pts',(-0.139836317888043,-0.203463743702801,
0.971100730005489));
#9484=CARTESIAN_POINT('Ctrl Pts',(-0.104422493053067,-0.224161999508995,
0.975530745318961));
#9485=CARTESIAN_POINT('Ctrl Pts',(-0.0842175114474176,-0.232861760990032,
0.977553872336861));
#9486=CARTESIAN_POINT('Ctrl Pts',(-0.0421062857595701,-0.244251601209411,
0.980270995488453));
#9487=CARTESIAN_POINT('Ctrl Pts',(-0.0201990724523197,-0.246942143572133,
0.980948));
#9488=CARTESIAN_POINT('Ctrl Pts',(0.020199072452319,-0.246942143572133,
0.980948));
#9489=CARTESIAN_POINT('Ctrl Pts',(0.0421062857595694,-0.244251601209411,
0.980270995488454));
#9490=CARTESIAN_POINT('Ctrl Pts',(0.0842175114474169,-0.232861760990032,
0.977553872336861));
#9491=CARTESIAN_POINT('Ctrl Pts',(0.104422493053067,-0.224161999508995,
0.975530745318961));
#9492=CARTESIAN_POINT('Ctrl Pts',(0.139836317888042,-0.203463743702801,
0.971100730005489));
#9493=CARTESIAN_POINT('Ctrl Pts',(0.15681442133453,-0.190326085855194,0.968453058988463));
#9494=CARTESIAN_POINT('Ctrl Pts',(0.1868781821531,-0.15976606450048,0.963103647174702));
#9495=CARTESIAN_POINT('Ctrl Pts',(0.199966927975188,-0.142345102874864,
0.960411259488514));
#9496=CARTESIAN_POINT('Ctrl Pts',(0.223801617934945,-0.0999305678883309,
0.955173119738174));
#9497=CARTESIAN_POINT('Ctrl Pts',(0.233157223576061,-0.0740444353928835,
0.952850216871763));
#9498=CARTESIAN_POINT('Ctrl Pts',(0.238183666596899,-0.0476299999999999,
0.951592097314));
#9499=CARTESIAN_POINT('Origin',(-1.94289029309402E-16,-0.04763,1.));
#9500=CARTESIAN_POINT('Origin',(0.,-0.04763,0.));
#9501=CARTESIAN_POINT('',(-0.504455939115715,-0.04763,0.841298510752802));
#9502=CARTESIAN_POINT('Origin',(0.,-0.04763,0.));
#9503=CARTESIAN_POINT('Origin',(-0.707106781186548,-0.04763,0.707106781186547));
#9504=CARTESIAN_POINT('Origin',(-0.707106781186548,0.,0.707106781186547));
#9505=CARTESIAN_POINT('',(-0.841298510752802,-0.04763,0.504455939115715));
#9506=CARTESIAN_POINT('Ctrl Pts',(-0.841298510752802,-0.04763,0.504455939115715));
#9507=CARTESIAN_POINT('Ctrl Pts',(-0.838633903678357,-0.0740444353928835,
0.508899795931835));
#9508=CARTESIAN_POINT('Ctrl Pts',(-0.833661031856294,-0.0999305678883309,
0.517157748491652));
#9509=CARTESIAN_POINT('Ctrl Pts',(-0.820511285096538,-0.142345102874864,
0.537715343527944));
#9510=CARTESIAN_POINT('Ctrl Pts',(-0.813159949759,-0.159766064500479,0.548874290046456));
#9511=CARTESIAN_POINT('Ctrl Pts',(-0.795684265985089,-0.190326085855194,
0.573915184558107));
#9512=CARTESIAN_POINT('Ctrl Pts',(-0.78555112003688,-0.203463743702801,
0.587792702767295));
#9513=CARTESIAN_POINT('Ctrl Pts',(-0.763642258217233,-0.224161999508995,
0.615966552324775));
#9514=CARTESIAN_POINT('Ctrl Pts',(-0.750785745543687,-0.232861760990032,
0.631684198665438));
#9515=CARTESIAN_POINT('Ctrl Pts',(-0.722929908501543,-0.244251601209411,
0.663382628119203));
#9516=CARTESIAN_POINT('Ctrl Pts',(-0.707917883896095,-0.246942143572133,
0.679352081686668));
#9517=CARTESIAN_POINT('Ctrl Pts',(-0.679352081686668,-0.246942143572133,
0.707917883896095));
#9518=CARTESIAN_POINT('Ctrl Pts',(-0.663382628119203,-0.244251601209411,
0.722929908501544));
#9519=CARTESIAN_POINT('Ctrl Pts',(-0.631684198665438,-0.232861760990031,
0.750785745543687));
#9520=CARTESIAN_POINT('Ctrl Pts',(-0.615966552324775,-0.224161999508995,
0.763642258217233));
#9521=CARTESIAN_POINT('Ctrl Pts',(-0.587792702767295,-0.203463743702801,
0.78555112003688));
#9522=CARTESIAN_POINT('Ctrl Pts',(-0.573915184558107,-0.190326085855194,
0.795684265985088));
#9523=CARTESIAN_POINT('Ctrl Pts',(-0.548874290046456,-0.159766064500479,
0.813159949759));
#9524=CARTESIAN_POINT('Ctrl Pts',(-0.537715343527944,-0.142345102874864,
0.820511285096538));
#9525=CARTESIAN_POINT('Ctrl Pts',(-0.517157748491652,-0.0999305678883309,
0.833661031856294));
#9526=CARTESIAN_POINT('Ctrl Pts',(-0.508899795931835,-0.0740444353928835,
0.838633903678357));
#9527=CARTESIAN_POINT('Ctrl Pts',(-0.504455939115716,-0.04763,0.841298510752801));
#9528=CARTESIAN_POINT('Origin',(-0.707106781186548,-0.04763,0.707106781186547));
#9529=CARTESIAN_POINT('Origin',(0.,-0.04763,0.));
#9530=CARTESIAN_POINT('',(-0.951592097314,-0.04763,0.238183666596899));
#9531=CARTESIAN_POINT('Origin',(0.,-0.04763,0.));
#9532=CARTESIAN_POINT('Origin',(-1.,-0.04763,-1.11022302462516E-16));
#9533=CARTESIAN_POINT('Origin',(-1.,0.,-1.11022302462516E-16));
#9534=CARTESIAN_POINT('',(-0.951592097314,-0.04763,-0.2381836665969));
#9535=CARTESIAN_POINT('',(-0.980948,-0.246942143572133,1.08514323328844E-18));
#9536=CARTESIAN_POINT('Ctrl Pts',(-0.951592097314,-0.04763,-0.238183666596899));
#9537=CARTESIAN_POINT('Ctrl Pts',(-0.952850216871763,-0.0740444353928835,
-0.233157223576062));
#9538=CARTESIAN_POINT('Ctrl Pts',(-0.955173119738174,-0.0999305678883309,
-0.223801617934946));
#9539=CARTESIAN_POINT('Ctrl Pts',(-0.960411259488514,-0.142345102874864,
-0.199966927975188));
#9540=CARTESIAN_POINT('Ctrl Pts',(-0.963103647174702,-0.159766064500479,
-0.1868781821531));
#9541=CARTESIAN_POINT('Ctrl Pts',(-0.968453058988463,-0.190326085855194,
-0.15681442133453));
#9542=CARTESIAN_POINT('Ctrl Pts',(-0.971100730005489,-0.203463743702801,
-0.139836317888043));
#9543=CARTESIAN_POINT('Ctrl Pts',(-0.975530745318961,-0.224161999508995,
-0.104422493053067));
#9544=CARTESIAN_POINT('Ctrl Pts',(-0.977553872336861,-0.232861760990032,
-0.0842175114474175));
#9545=CARTESIAN_POINT('Ctrl Pts',(-0.980270995488453,-0.244251601209411,
-0.0421062857595699));
#9546=CARTESIAN_POINT('Ctrl Pts',(-0.980948,-0.246942143572133,-0.0201990724523195));
#9547=CARTESIAN_POINT('Ctrl Pts',(-0.980948,-0.246942143572133,-1.17961196366423E-16));
#9548=CARTESIAN_POINT('Origin',(-1.,-0.04763,-1.11022302462516E-16));
#9549=CARTESIAN_POINT('Ctrl Pts',(-0.980948,-0.246942143572133,-1.17961196366423E-16));
#9550=CARTESIAN_POINT('Ctrl Pts',(-0.980948,-0.246942143572133,0.0201990724523192));
#9551=CARTESIAN_POINT('Ctrl Pts',(-0.980270995488453,-0.244251601209411,
0.0421062857595695));
#9552=CARTESIAN_POINT('Ctrl Pts',(-0.977553872336861,-0.232861760990032,
0.0842175114474169));
#9553=CARTESIAN_POINT('Ctrl Pts',(-0.975530745318961,-0.224161999508995,
0.104422493053066));
#9554=CARTESIAN_POINT('Ctrl Pts',(-0.971100730005489,-0.203463743702801,
0.139836317888042));
#9555=CARTESIAN_POINT('Ctrl Pts',(-0.968453058988463,-0.190326085855194,
0.15681442133453));
#9556=CARTESIAN_POINT('Ctrl Pts',(-0.963103647174702,-0.15976606450048,
0.1868781821531));
#9557=CARTESIAN_POINT('Ctrl Pts',(-0.960411259488514,-0.142345102874864,
0.199966927975188));
#9558=CARTESIAN_POINT('Ctrl Pts',(-0.955173119738174,-0.099930567888331,
0.223801617934945));
#9559=CARTESIAN_POINT('Ctrl Pts',(-0.952850216871763,-0.0740444353928835,
0.233157223576061));
#9560=CARTESIAN_POINT('Ctrl Pts',(-0.951592097314,-0.04763,0.238183666596899));
#9561=CARTESIAN_POINT('Origin',(0.,-0.04763,0.));
#9562=CARTESIAN_POINT('',(-0.841298510752802,-0.04763,-0.504455939115715));
#9563=CARTESIAN_POINT('Origin',(0.,-0.04763,0.));
#9564=CARTESIAN_POINT('Origin',(-0.707106781186547,-0.04763,-0.707106781186548));
#9565=CARTESIAN_POINT('Origin',(-0.707106781186547,0.,-0.707106781186548));
#9566=CARTESIAN_POINT('',(-0.504455939115715,-0.04763,-0.841298510752802));
#9567=CARTESIAN_POINT('Ctrl Pts',(-0.504455939115715,-0.04763,-0.841298510752802));
#9568=CARTESIAN_POINT('Ctrl Pts',(-0.508899795931835,-0.0740444353928835,
-0.838633903678357));
#9569=CARTESIAN_POINT('Ctrl Pts',(-0.517157748491652,-0.0999305678883309,
-0.833661031856294));
#9570=CARTESIAN_POINT('Ctrl Pts',(-0.537715343527944,-0.142345102874864,
-0.820511285096538));
#9571=CARTESIAN_POINT('Ctrl Pts',(-0.548874290046456,-0.159766064500479,
-0.813159949759));
#9572=CARTESIAN_POINT('Ctrl Pts',(-0.573915184558107,-0.190326085855194,
-0.795684265985089));
#9573=CARTESIAN_POINT('Ctrl Pts',(-0.587792702767295,-0.203463743702801,
-0.78555112003688));
#9574=CARTESIAN_POINT('Ctrl Pts',(-0.615966552324775,-0.224161999508995,
-0.763642258217233));
#9575=CARTESIAN_POINT('Ctrl Pts',(-0.631684198665438,-0.232861760990032,
-0.750785745543687));
#9576=CARTESIAN_POINT('Ctrl Pts',(-0.663382628119203,-0.244251601209411,
-0.722929908501543));
#9577=CARTESIAN_POINT('Ctrl Pts',(-0.679352081686668,-0.246942143572133,
-0.707917883896095));
#9578=CARTESIAN_POINT('Ctrl Pts',(-0.707917883896095,-0.246942143572133,
-0.679352081686668));
#9579=CARTESIAN_POINT('Ctrl Pts',(-0.722929908501543,-0.244251601209411,
-0.663382628119203));
#9580=CARTESIAN_POINT('Ctrl Pts',(-0.750785745543687,-0.232861760990032,
-0.631684198665439));
#9581=CARTESIAN_POINT('Ctrl Pts',(-0.763642258217232,-0.224161999508995,
-0.615966552324775));
#9582=CARTESIAN_POINT('Ctrl Pts',(-0.78555112003688,-0.203463743702801,
-0.587792702767295));
#9583=CARTESIAN_POINT('Ctrl Pts',(-0.795684265985088,-0.190326085855194,
-0.573915184558107));
#9584=CARTESIAN_POINT('Ctrl Pts',(-0.813159949759,-0.15976606450048,-0.548874290046456));
#9585=CARTESIAN_POINT('Ctrl Pts',(-0.820511285096538,-0.142345102874864,
-0.537715343527944));
#9586=CARTESIAN_POINT('Ctrl Pts',(-0.833661031856294,-0.0999305678883311,
-0.517157748491652));
#9587=CARTESIAN_POINT('Ctrl Pts',(-0.838633903678357,-0.0740444353928836,
-0.508899795931835));
#9588=CARTESIAN_POINT('Ctrl Pts',(-0.841298510752801,-0.04763,-0.504455939115715));
#9589=CARTESIAN_POINT('Origin',(-0.707106781186547,-0.04763,-0.707106781186548));
#9590=CARTESIAN_POINT('Origin',(0.,-0.04763,0.));
#9591=CARTESIAN_POINT('',(-0.238183666596899,-0.04763,-0.951592097314));
#9592=CARTESIAN_POINT('Origin',(0.,-0.04763,0.));
#9593=CARTESIAN_POINT('Origin',(5.55111512312578E-17,-0.04763,-1.));
#9594=CARTESIAN_POINT('Origin',(5.55111512312578E-17,0.,-1.));
#9595=CARTESIAN_POINT('',(0.238183666596899,-0.04763,-0.951592097314));
#9596=CARTESIAN_POINT('Ctrl Pts',(0.238183666596899,-0.04763,-0.951592097314));
#9597=CARTESIAN_POINT('Ctrl Pts',(0.233157223576062,-0.0740444353928835,
-0.952850216871763));
#9598=CARTESIAN_POINT('Ctrl Pts',(0.223801617934946,-0.099930567888331,
-0.955173119738174));
#9599=CARTESIAN_POINT('Ctrl Pts',(0.199966927975188,-0.142345102874864,
-0.960411259488514));
#9600=CARTESIAN_POINT('Ctrl Pts',(0.1868781821531,-0.15976606450048,-0.963103647174702));
#9601=CARTESIAN_POINT('Ctrl Pts',(0.15681442133453,-0.190326085855194,-0.968453058988463));
#9602=CARTESIAN_POINT('Ctrl Pts',(0.139836317888042,-0.203463743702801,
-0.971100730005489));
#9603=CARTESIAN_POINT('Ctrl Pts',(0.104422493053067,-0.224161999508995,
-0.975530745318961));
#9604=CARTESIAN_POINT('Ctrl Pts',(0.0842175114474173,-0.232861760990032,
-0.977553872336861));
#9605=CARTESIAN_POINT('Ctrl Pts',(0.0421062857595698,-0.244251601209411,
-0.980270995488453));
#9606=CARTESIAN_POINT('Ctrl Pts',(0.0201990724523194,-0.246942143572133,
-0.980948));
#9607=CARTESIAN_POINT('Ctrl Pts',(-0.0201990724523193,-0.246942143572133,
-0.980948));
#9608=CARTESIAN_POINT('Ctrl Pts',(-0.0421062857595697,-0.244251601209411,
-0.980270995488453));
#9609=CARTESIAN_POINT('Ctrl Pts',(-0.0842175114474171,-0.232861760990032,
-0.977553872336861));
#9610=CARTESIAN_POINT('Ctrl Pts',(-0.104422493053067,-0.224161999508995,
-0.975530745318961));
#9611=CARTESIAN_POINT('Ctrl Pts',(-0.139836317888042,-0.203463743702801,
-0.971100730005489));
#9612=CARTESIAN_POINT('Ctrl Pts',(-0.15681442133453,-0.190326085855194,
-0.968453058988463));
#9613=CARTESIAN_POINT('Ctrl Pts',(-0.1868781821531,-0.15976606450048,-0.963103647174702));
#9614=CARTESIAN_POINT('Ctrl Pts',(-0.199966927975188,-0.142345102874864,
-0.960411259488514));
#9615=CARTESIAN_POINT('Ctrl Pts',(-0.223801617934945,-0.099930567888331,
-0.955173119738174));
#9616=CARTESIAN_POINT('Ctrl Pts',(-0.233157223576062,-0.0740444353928835,
-0.952850216871763));
#9617=CARTESIAN_POINT('Ctrl Pts',(-0.238183666596899,-0.0476299999999999,
-0.951592097314));
#9618=CARTESIAN_POINT('Origin',(5.55111512312578E-17,-0.04763,-1.));
#9619=CARTESIAN_POINT('Origin',(0.,-0.04763,0.));
#9620=CARTESIAN_POINT('',(0.504455939115715,-0.04763,-0.841298510752802));
#9621=CARTESIAN_POINT('Origin',(0.,-0.04763,0.));
#9622=CARTESIAN_POINT('Origin',(0.707106781186548,-0.04763,-0.707106781186547));
#9623=CARTESIAN_POINT('Origin',(0.707106781186548,0.,-0.707106781186547));
#9624=CARTESIAN_POINT('',(0.841298510752802,-0.04763,-0.504455939115715));
#9625=CARTESIAN_POINT('Ctrl Pts',(0.841298510752802,-0.04763,-0.504455939115715));
#9626=CARTESIAN_POINT('Ctrl Pts',(0.838633903678357,-0.0740444353928835,
-0.508899795931835));
#9627=CARTESIAN_POINT('Ctrl Pts',(0.833661031856294,-0.0999305678883309,
-0.517157748491652));
#9628=CARTESIAN_POINT('Ctrl Pts',(0.820511285096538,-0.142345102874864,
-0.537715343527944));
#9629=CARTESIAN_POINT('Ctrl Pts',(0.813159949759,-0.159766064500479,-0.548874290046456));
#9630=CARTESIAN_POINT('Ctrl Pts',(0.795684265985088,-0.190326085855194,
-0.573915184558107));
#9631=CARTESIAN_POINT('Ctrl Pts',(0.78555112003688,-0.203463743702801,-0.587792702767295));
#9632=CARTESIAN_POINT('Ctrl Pts',(0.763642258217233,-0.224161999508995,
-0.615966552324775));
#9633=CARTESIAN_POINT('Ctrl Pts',(0.750785745543687,-0.232861760990032,
-0.631684198665438));
#9634=CARTESIAN_POINT('Ctrl Pts',(0.722929908501543,-0.244251601209411,
-0.663382628119203));
#9635=CARTESIAN_POINT('Ctrl Pts',(0.707917883896095,-0.246942143572133,
-0.679352081686668));
#9636=CARTESIAN_POINT('Ctrl Pts',(0.679352081686668,-0.246942143572133,
-0.707917883896095));
#9637=CARTESIAN_POINT('Ctrl Pts',(0.663382628119203,-0.244251601209411,
-0.722929908501543));
#9638=CARTESIAN_POINT('Ctrl Pts',(0.631684198665438,-0.232861760990032,
-0.750785745543687));
#9639=CARTESIAN_POINT('Ctrl Pts',(0.615966552324775,-0.224161999508995,
-0.763642258217232));
#9640=CARTESIAN_POINT('Ctrl Pts',(0.587792702767295,-0.203463743702801,
-0.78555112003688));
#9641=CARTESIAN_POINT('Ctrl Pts',(0.573915184558107,-0.190326085855194,
-0.795684265985088));
#9642=CARTESIAN_POINT('Ctrl Pts',(0.548874290046456,-0.159766064500479,
-0.813159949759));
#9643=CARTESIAN_POINT('Ctrl Pts',(0.537715343527944,-0.142345102874864,
-0.820511285096538));
#9644=CARTESIAN_POINT('Ctrl Pts',(0.517157748491652,-0.099930567888331,
-0.833661031856294));
#9645=CARTESIAN_POINT('Ctrl Pts',(0.508899795931835,-0.0740444353928835,
-0.838633903678357));
#9646=CARTESIAN_POINT('Ctrl Pts',(0.504455939115715,-0.04763,-0.841298510752801));
#9647=CARTESIAN_POINT('Origin',(0.707106781186548,-0.04763,-0.707106781186547));
#9648=CARTESIAN_POINT('Origin',(0.,-0.166705,0.));
#9649=CARTESIAN_POINT('',(-0.980948,-0.28578,1.20131482833E-16));
#9650=CARTESIAN_POINT('Origin',(0.,-0.28578,0.));
#9651=CARTESIAN_POINT('',(-0.980948,-0.166705,1.20131482833E-16));
#9652=CARTESIAN_POINT('',(0.951592097314,-0.04763,0.238183666596899));
#9653=CARTESIAN_POINT('Origin',(0.,-0.04763,0.));
#9654=CARTESIAN_POINT('',(0.951592097314,-0.04763,-0.238183666596899));
#9655=CARTESIAN_POINT('Ctrl Pts',(0.951592097314,-0.04763,0.238183666596899));
#9656=CARTESIAN_POINT('Ctrl Pts',(0.952850216871763,-0.0740444353928835,
0.233157223576062));
#9657=CARTESIAN_POINT('Ctrl Pts',(0.955173119738174,-0.099930567888331,
0.223801617934945));
#9658=CARTESIAN_POINT('Ctrl Pts',(0.960411259488514,-0.142345102874864,
0.199966927975188));
#9659=CARTESIAN_POINT('Ctrl Pts',(0.963103647174702,-0.15976606450048,0.1868781821531));
#9660=CARTESIAN_POINT('Ctrl Pts',(0.968453058988463,-0.190326085855194,
0.15681442133453));
#9661=CARTESIAN_POINT('Ctrl Pts',(0.971100730005489,-0.203463743702801,
0.139836317888042));
#9662=CARTESIAN_POINT('Ctrl Pts',(0.975530745318961,-0.224161999508995,
0.104422493053067));
#9663=CARTESIAN_POINT('Ctrl Pts',(0.977553872336861,-0.232861760990032,
0.0842175114474172));
#9664=CARTESIAN_POINT('Ctrl Pts',(0.980270995488453,-0.244251601209411,
0.0421062857595697));
#9665=CARTESIAN_POINT('Ctrl Pts',(0.980948,-0.246942143572133,0.0201990724523194));
#9666=CARTESIAN_POINT('Ctrl Pts',(0.980948,-0.246942143572133,-0.0201990724523194));
#9667=CARTESIAN_POINT('Ctrl Pts',(0.980270995488453,-0.244251601209411,
-0.0421062857595697));
#9668=CARTESIAN_POINT('Ctrl Pts',(0.977553872336861,-0.232861760990032,
-0.0842175114474172));
#9669=CARTESIAN_POINT('Ctrl Pts',(0.975530745318961,-0.224161999508995,
-0.104422493053067));
#9670=CARTESIAN_POINT('Ctrl Pts',(0.971100730005489,-0.203463743702801,
-0.139836317888042));
#9671=CARTESIAN_POINT('Ctrl Pts',(0.968453058988463,-0.190326085855194,
-0.15681442133453));
#9672=CARTESIAN_POINT('Ctrl Pts',(0.963103647174702,-0.15976606450048,-0.1868781821531));
#9673=CARTESIAN_POINT('Ctrl Pts',(0.960411259488514,-0.142345102874864,
-0.199966927975188));
#9674=CARTESIAN_POINT('Ctrl Pts',(0.955173119738174,-0.099930567888331,
-0.223801617934945));
#9675=CARTESIAN_POINT('Ctrl Pts',(0.952850216871763,-0.0740444353928835,
-0.233157223576062));
#9676=CARTESIAN_POINT('Ctrl Pts',(0.951592097314,-0.0476299999999999,-0.238183666596899));
#9677=CARTESIAN_POINT('Origin',(0.,-0.04763,0.));
#9678=CARTESIAN_POINT('Origin',(0.,-0.04763,0.));
#9679=CARTESIAN_POINT('Origin',(1.,-0.04763,0.));
#9680=CARTESIAN_POINT('Origin',(1.,0.,0.));
#9681=CARTESIAN_POINT('Origin',(1.,-0.04763,0.));
#9682=CARTESIAN_POINT('Origin',(0.,-0.28578,0.));
#9683=CARTESIAN_POINT('Origin',(0.,-0.04763,0.));
#9684=CARTESIAN_POINT('',(0.,0.,0.));
#9685=CARTESIAN_POINT('Origin',(1.013815,0.445,0.));
#9686=CARTESIAN_POINT('',(-1.013815,0.445,-1.24156529467757E-16));
#9687=CARTESIAN_POINT('Origin',(0.,0.445,0.));
#9688=CARTESIAN_POINT('',(-0.991185,0.445,-1.21385153761287E-16));
#9689=CARTESIAN_POINT('Origin',(0.,0.445,0.));
#9690=CARTESIAN_POINT('Origin',(0.,0.4075,0.));
#9691=CARTESIAN_POINT('',(-1.013815,0.37,-1.24156529467757E-16));
#9692=CARTESIAN_POINT('Origin',(0.,0.37,0.));
#9693=CARTESIAN_POINT('',(-1.013815,0.4075,-1.24156529467757E-16));
#9694=CARTESIAN_POINT('Origin',(0.991185,0.37,0.));
#9695=CARTESIAN_POINT('',(-0.991185,0.37,-1.21385153761287E-16));
#9696=CARTESIAN_POINT('Origin',(0.,0.37,0.));
#9697=CARTESIAN_POINT('Origin',(0.,0.4075,0.));
#9698=CARTESIAN_POINT('',(-0.991185,0.4075,-1.21385153761287E-16));
#9699=CARTESIAN_POINT('Origin',(1.013815,-0.37,0.));
#9700=CARTESIAN_POINT('',(-1.013815,-0.37,-1.24156529467757E-16));
#9701=CARTESIAN_POINT('Origin',(0.,-0.37,0.));
#9702=CARTESIAN_POINT('',(-0.991185,-0.37,-1.21385153761287E-16));
#9703=CARTESIAN_POINT('Origin',(0.,-0.37,0.));
#9704=CARTESIAN_POINT('Origin',(0.,-0.4075,0.));
#9705=CARTESIAN_POINT('',(-1.013815,-0.445,-1.24156529467757E-16));
#9706=CARTESIAN_POINT('Origin',(0.,-0.445,0.));
#9707=CARTESIAN_POINT('',(-1.013815,-0.4075,-1.24156529467757E-16));
#9708=CARTESIAN_POINT('Origin',(0.991185,-0.445,0.));
#9709=CARTESIAN_POINT('',(-0.991185,-0.445,-1.21385153761287E-16));
#9710=CARTESIAN_POINT('Origin',(0.,-0.445,0.));
#9711=CARTESIAN_POINT('Origin',(0.,-0.4075,0.));
#9712=CARTESIAN_POINT('',(-0.991185,-0.4075,-1.21385153761287E-16));
#9713=CARTESIAN_POINT('',(0.,0.,0.));
#9714=CARTESIAN_POINT('',(0.,0.,0.));
#9715=CARTESIAN_POINT('',(0.,0.,0.));
#9716=CARTESIAN_POINT('',(0.,0.,0.));
#9717=CARTESIAN_POINT('',(0.,0.,0.));
#9718=CARTESIAN_POINT('',(0.,0.,0.));
#9719=CARTESIAN_POINT('',(0.,0.,0.));
#9720=CARTESIAN_POINT('Origin',(0.,0.,5.9));
#9721=CARTESIAN_POINT('',(-0.165,-2.02066721859313E-17,5.9));
#9722=CARTESIAN_POINT('Origin',(0.,0.,5.9));
#9723=CARTESIAN_POINT('',(-0.165,2.02066721859313E-17,6.8));
#9724=CARTESIAN_POINT('',(-0.165,-2.02066721859313E-17,5.9));
#9725=CARTESIAN_POINT('Origin',(0.,0.,6.8));
#9726=CARTESIAN_POINT('Origin',(0.,0.,5.9));
#9727=CARTESIAN_POINT('Origin',(3.,0.,4.7));
#9728=CARTESIAN_POINT('',(2.75,-3.06161699786838E-17,4.8));
#9729=CARTESIAN_POINT('Origin',(3.,0.,4.8));
#9730=CARTESIAN_POINT('',(2.75,3.06161699786838E-17,5.2));
#9731=CARTESIAN_POINT('',(2.75,-3.06161699786838E-17,4.7));
#9732=CARTESIAN_POINT('Origin',(3.,0.,5.2));
#9733=CARTESIAN_POINT('Origin',(3.,0.,4.8));
#9734=CARTESIAN_POINT('',(3.,0.5,4.8));
#9735=CARTESIAN_POINT('',(3.,0.5,5.2));
#9736=CARTESIAN_POINT('',(3.,0.5,4.8));
#9737=CARTESIAN_POINT('',(3.,-0.5,5.2));
#9738=CARTESIAN_POINT('Origin',(3.,0.,5.2));
#9739=CARTESIAN_POINT('',(3.,-0.5,4.8));
#9740=CARTESIAN_POINT('',(3.,-0.5,4.8));
#9741=CARTESIAN_POINT('Origin',(3.,0.,4.8));
#9742=CARTESIAN_POINT('Origin',(0.,0.,4.8));
#9743=CARTESIAN_POINT('',(0.866025403784439,-0.5,4.8));
#9744=CARTESIAN_POINT('',(-2.5,-0.5,4.8));
#9745=CARTESIAN_POINT('',(-0.866025403784439,-0.5,4.8));
#9746=CARTESIAN_POINT('Origin',(0.,0.,4.8));
#9747=CARTESIAN_POINT('',(-2.5,-0.5,4.8));
#9748=CARTESIAN_POINT('',(-2.5,-0.5,4.8));
#9749=CARTESIAN_POINT('',(-2.5,0.5,4.8));
#9750=CARTESIAN_POINT('',(-2.5,0.5,4.8));
#9751=CARTESIAN_POINT('',(-0.866025403784439,0.5,4.8));
#9752=CARTESIAN_POINT('',(3.,0.5,4.8));
#9753=CARTESIAN_POINT('',(0.866025403784439,0.5,4.8));
#9754=CARTESIAN_POINT('Origin',(0.,0.,4.8));
#9755=CARTESIAN_POINT('',(3.,0.5,4.8));
#9756=CARTESIAN_POINT('',(-0.7,-8.57252759403147E-17,4.8));
#9757=CARTESIAN_POINT('Origin',(0.,0.,4.8));
#9758=CARTESIAN_POINT('Origin',(3.,0.5,4.8));
#9759=CARTESIAN_POINT('',(0.866025403784439,0.5,5.2));
#9760=CARTESIAN_POINT('',(0.866025403784439,0.5,4.8));
#9761=CARTESIAN_POINT('',(3.,0.5,5.2));
#9762=CARTESIAN_POINT('Origin',(-2.5,-0.5,4.8));
#9763=CARTESIAN_POINT('',(0.866025403784439,-0.5,5.2));
#9764=CARTESIAN_POINT('',(0.866025403784439,-0.5,4.8));
#9765=CARTESIAN_POINT('',(-2.5,-0.5,5.2));
#9766=CARTESIAN_POINT('Origin',(-2.5,-0.5,4.8));
#9767=CARTESIAN_POINT('',(-0.866025403784439,-0.5,5.2));
#9768=CARTESIAN_POINT('',(-0.866025403784439,-0.5,4.8));
#9769=CARTESIAN_POINT('',(-2.5,-0.5,5.2));
#9770=CARTESIAN_POINT('',(-2.5,-0.5,5.2));
#9771=CARTESIAN_POINT('',(-2.5,-0.5,4.8));
#9772=CARTESIAN_POINT('Origin',(3.,0.5,4.8));
#9773=CARTESIAN_POINT('',(-0.866025403784439,0.5,5.2));
#9774=CARTESIAN_POINT('',(-0.866025403784439,0.5,4.8));
#9775=CARTESIAN_POINT('',(-2.5,0.5,5.2));
#9776=CARTESIAN_POINT('',(-2.5,0.5,4.8));
#9777=CARTESIAN_POINT('',(3.,0.5,5.2));
#9778=CARTESIAN_POINT('Origin',(-2.5,0.5,4.8));
#9779=CARTESIAN_POINT('',(-2.5,0.5,5.2));
#9780=CARTESIAN_POINT('Origin',(0.,0.,5.2));
#9781=CARTESIAN_POINT('Origin',(0.,0.,5.2));
#9782=CARTESIAN_POINT('Origin',(0.,0.,5.2));
#9783=CARTESIAN_POINT('',(-0.5,-6.12323399573677E-17,5.2));
#9784=CARTESIAN_POINT('Origin',(0.,0.,5.2));
#9785=CARTESIAN_POINT('Origin',(0.,0.,4.8));
#9786=CARTESIAN_POINT('Origin',(0.,0.,4.8));
#9787=CARTESIAN_POINT('Origin',(0.,0.,2.95));
#9788=CARTESIAN_POINT('',(-0.7,-8.57252759403147E-17,2.95));
#9789=CARTESIAN_POINT('Origin',(0.,0.,2.95));
#9790=CARTESIAN_POINT('',(-0.5,6.12323399573677E-17,2.95));
#9791=CARTESIAN_POINT('Origin',(0.,0.,2.95));
#9792=CARTESIAN_POINT('Origin',(0.,0.,2.95));
#9793=CARTESIAN_POINT('',(-0.7,-8.57252759403147E-17,2.95));
#9794=CARTESIAN_POINT('Origin',(0.,0.,1.));
#9795=CARTESIAN_POINT('',(-0.5,-6.12323399573677E-17,1.));
#9796=CARTESIAN_POINT('',(-0.5,-6.12323399573677E-17,1.));
#9797=CARTESIAN_POINT('Origin',(0.,0.,1.));
#9798=CARTESIAN_POINT('Origin',(0.,0.,1.));
#9799=CARTESIAN_POINT('',(-0.5,-6.12323399573677E-17,6.8));
#9800=CARTESIAN_POINT('Origin',(0.,0.,6.8));
#9801=CARTESIAN_POINT('',(-0.5,-6.12323399573677E-17,1.));
#9802=CARTESIAN_POINT('Origin',(0.,0.,6.8));
#9803=CARTESIAN_POINT('Origin',(0.,0.,1.));
#9804=CARTESIAN_POINT('',(0.,0.,0.));
#9805=CARTESIAN_POINT('Origin',(0.,0.,1.8));
#9806=CARTESIAN_POINT('',(-0.505,-6.18446633569413E-17,2.05));
#9807=CARTESIAN_POINT('Origin',(0.,0.,2.05));
#9808=CARTESIAN_POINT('',(-0.505,-6.18446633569413E-17,1.8));
#9809=CARTESIAN_POINT('',(-0.505,-6.18446633569413E-17,1.8));
#9810=CARTESIAN_POINT('Origin',(0.,0.,1.8));
#9811=CARTESIAN_POINT('Origin',(0.,0.,1.8));
#9812=CARTESIAN_POINT('',(-0.7,-8.57252759403147E-17,2.05));
#9813=CARTESIAN_POINT('Origin',(0.,0.,2.05));
#9814=CARTESIAN_POINT('',(-0.7,-8.57252759403147E-17,1.8));
#9815=CARTESIAN_POINT('',(-0.7,-8.57252759403147E-17,1.8));
#9816=CARTESIAN_POINT('Origin',(0.,0.,1.8));
#9817=CARTESIAN_POINT('Origin',(0.,0.,2.05));
#9818=CARTESIAN_POINT('Origin',(0.,0.,1.8));
#9819=CARTESIAN_POINT('',(0.,0.,0.));
#9820=CARTESIAN_POINT('Origin',(0.,-0.49,1.4));
#9821=CARTESIAN_POINT('',(-0.122167917228706,-0.49,1.51090536506409));
#9822=CARTESIAN_POINT('',(-0.122167917228706,-0.49,1.28909463493591));
#9823=CARTESIAN_POINT('',(-0.122167917228706,-0.49,1.));
#9824=CARTESIAN_POINT('',(-0.165,-0.49,1.4));
#9825=CARTESIAN_POINT('Origin',(0.,-0.49,1.4));
#9826=CARTESIAN_POINT('Origin',(0.,-0.49,1.4));
#9827=CARTESIAN_POINT('Origin',(0.,-1.,1.4));
#9828=CARTESIAN_POINT('',(-0.165,-0.884745726183518,1.4));
#9829=CARTESIAN_POINT('Ctrl Pts',(-0.165,-0.884745726183518,1.4));
#9830=CARTESIAN_POINT('Ctrl Pts',(-0.165,-0.884745726183518,1.42076875940744));
#9831=CARTESIAN_POINT('Ctrl Pts',(-0.160839719007584,-0.885552759505264,
1.44288889507334));
#9832=CARTESIAN_POINT('Ctrl Pts',(-0.14398647021669,-0.888448648150043,
1.48352706263377));
#9833=CARTESIAN_POINT('Ctrl Pts',(-0.131295993814186,-0.890493604851638,
1.50204924397737));
#9834=CARTESIAN_POINT('Ctrl Pts',(-0.102049819008125,-0.89431723432394,
1.53129541878344));
#9835=CARTESIAN_POINT('Ctrl Pts',(-0.0835273920906823,-0.896347088899543,
1.54398634598358));
#9836=CARTESIAN_POINT('Ctrl Pts',(-0.0428883760934128,-0.899208271860583,
1.56083992183864));
#9837=CARTESIAN_POINT('Ctrl Pts',(-0.0207679427235068,-0.9,1.565));
#9838=CARTESIAN_POINT('Ctrl Pts',(0.0207679427235068,-0.9,1.565));
#9839=CARTESIAN_POINT('Ctrl Pts',(0.0428883760934127,-0.899208271860583,
1.56083992183864));
#9840=CARTESIAN_POINT('Ctrl Pts',(0.0835273920906823,-0.896347088899543,
1.54398634598358));
#9841=CARTESIAN_POINT('Ctrl Pts',(0.102049819008125,-0.89431723432394,1.53129541878344));
#9842=CARTESIAN_POINT('Ctrl Pts',(0.131295993814186,-0.890493604851638,
1.50204924397737));
#9843=CARTESIAN_POINT('Ctrl Pts',(0.14398647021669,-0.888448648150043,1.48352706263377));
#9844=CARTESIAN_POINT('Ctrl Pts',(0.160839719007584,-0.885552759505264,
1.44288889507334));
#9845=CARTESIAN_POINT('Ctrl Pts',(0.165,-0.884745726183518,1.42076875940744));
#9846=CARTESIAN_POINT('Ctrl Pts',(0.165,-0.884745726183518,1.37923124059256));
#9847=CARTESIAN_POINT('Ctrl Pts',(0.160839719007584,-0.885552759505264,
1.35711110492666));
#9848=CARTESIAN_POINT('Ctrl Pts',(0.14398647021669,-0.888448648150043,1.31647293736623));
#9849=CARTESIAN_POINT('Ctrl Pts',(0.131295993814186,-0.890493604851638,
1.29795075602263));
#9850=CARTESIAN_POINT('Ctrl Pts',(0.102049819008125,-0.89431723432394,1.26870458121656));
#9851=CARTESIAN_POINT('Ctrl Pts',(0.0835273920906823,-0.896347088899543,
1.25601365401642));
#9852=CARTESIAN_POINT('Ctrl Pts',(0.0428883760934127,-0.899208271860583,
1.23916007816136));
#9853=CARTESIAN_POINT('Ctrl Pts',(0.0207679427235068,-0.9,1.235));
#9854=CARTESIAN_POINT('Ctrl Pts',(-0.0207679427235067,-0.9,1.235));
#9855=CARTESIAN_POINT('Ctrl Pts',(-0.0428883760934127,-0.899208271860583,
1.23916007816136));
#9856=CARTESIAN_POINT('Ctrl Pts',(-0.0835273920906822,-0.896347088899543,
1.25601365401642));
#9857=CARTESIAN_POINT('Ctrl Pts',(-0.102049819008125,-0.89431723432394,
1.26870458121656));
#9858=CARTESIAN_POINT('Ctrl Pts',(-0.131295993814186,-0.890493604851638,
1.29795075602263));
#9859=CARTESIAN_POINT('Ctrl Pts',(-0.14398647021669,-0.888448648150043,
1.31647293736623));
#9860=CARTESIAN_POINT('Ctrl Pts',(-0.160839719007584,-0.885552759505264,
1.35711110492666));
#9861=CARTESIAN_POINT('Ctrl Pts',(-0.165,-0.884745726183518,1.37923124059256));
#9862=CARTESIAN_POINT('Ctrl Pts',(-0.165,-0.884745726183518,1.4));
#9863=CARTESIAN_POINT('',(-0.165,-1.,1.4));
#9864=CARTESIAN_POINT('',(0.122167917228706,-0.49,1.51090536506409));
#9865=CARTESIAN_POINT('Ctrl Pts',(0.122167917228706,-0.49,1.51090536506409));
#9866=CARTESIAN_POINT('Ctrl Pts',(0.120368913626296,-0.490448531679987,
1.51288705930464));
#9867=CARTESIAN_POINT('Ctrl Pts',(0.118534896565231,-0.490895245371684,
1.51481034122633));
#9868=CARTESIAN_POINT('Ctrl Pts',(0.102111993019358,-0.494795015531646,
1.5312332447722));
#9869=CARTESIAN_POINT('Ctrl Pts',(0.0836597150224318,-0.498442514607594,
1.54390845611142));
#9870=CARTESIAN_POINT('Ctrl Pts',(0.0430495960471595,-0.50357781976106,
1.56079590960766));
#9871=CARTESIAN_POINT('Ctrl Pts',(0.020880094330741,-0.505,1.565));
#9872=CARTESIAN_POINT('Ctrl Pts',(-0.020880094330741,-0.505,1.565));
#9873=CARTESIAN_POINT('Ctrl Pts',(-0.0430495960471594,-0.50357781976106,
1.56079590960766));
#9874=CARTESIAN_POINT('Ctrl Pts',(-0.0836597150224317,-0.498442514607594,
1.54390845611142));
#9875=CARTESIAN_POINT('Ctrl Pts',(-0.102111993019358,-0.494795015531646,
1.5312332447722));
#9876=CARTESIAN_POINT('Ctrl Pts',(-0.118534896565231,-0.490895245371684,
1.51481034122633));
#9877=CARTESIAN_POINT('Ctrl Pts',(-0.120368913626296,-0.490448531679987,
1.51288705930464));
#9878=CARTESIAN_POINT('Ctrl Pts',(-0.122167917228706,-0.49,1.51090536506409));
#9879=CARTESIAN_POINT('',(0.122167917228706,-0.49,1.28909463493591));
#9880=CARTESIAN_POINT('Origin',(0.,-0.49,1.4));
#9881=CARTESIAN_POINT('Ctrl Pts',(-0.122167917228706,-0.49,1.28909463493591));
#9882=CARTESIAN_POINT('Ctrl Pts',(-0.120368913626296,-0.490448531679987,
1.28711294069536));
#9883=CARTESIAN_POINT('Ctrl Pts',(-0.118534896565231,-0.490895245371684,
1.28518965877367));
#9884=CARTESIAN_POINT('Ctrl Pts',(-0.102111993019358,-0.494795015531646,
1.2687667552278));
#9885=CARTESIAN_POINT('Ctrl Pts',(-0.0836597150224318,-0.498442514607594,
1.25609154388858));
#9886=CARTESIAN_POINT('Ctrl Pts',(-0.0430495960471595,-0.50357781976106,
1.23920409039234));
#9887=CARTESIAN_POINT('Ctrl Pts',(-0.020880094330741,-0.505,1.235));
#9888=CARTESIAN_POINT('Ctrl Pts',(0.020880094330741,-0.505,1.235));
#9889=CARTESIAN_POINT('Ctrl Pts',(0.0430495960471595,-0.50357781976106,
1.23920409039234));
#9890=CARTESIAN_POINT('Ctrl Pts',(0.0836597150224318,-0.498442514607594,
1.25609154388858));
#9891=CARTESIAN_POINT('Ctrl Pts',(0.102111993019358,-0.494795015531646,
1.2687667552278));
#9892=CARTESIAN_POINT('Ctrl Pts',(0.118534896565231,-0.490895245371684,
1.28518965877367));
#9893=CARTESIAN_POINT('Ctrl Pts',(0.120368913626296,-0.490448531679987,
1.28711294069536));
#9894=CARTESIAN_POINT('Ctrl Pts',(0.122167917228706,-0.49,1.28909463493591));
#9895=CARTESIAN_POINT('Origin',(0.,-0.49,1.4));
#9896=CARTESIAN_POINT('',(0.122167917228706,-0.49,1.));
#9897=CARTESIAN_POINT('Origin',(-0.49,0.,1.4));
#9898=CARTESIAN_POINT('',(-0.49,0.122167917228706,1.51090536506409));
#9899=CARTESIAN_POINT('',(-0.49,0.122167917228706,1.28909463493591));
#9900=CARTESIAN_POINT('',(-0.49,0.122167917228706,1.));
#9901=CARTESIAN_POINT('Origin',(-0.49,0.,1.4));
#9902=CARTESIAN_POINT('Origin',(-1.,0.,1.4));
#9903=CARTESIAN_POINT('',(-0.884745726183518,0.165,1.4));
#9904=CARTESIAN_POINT('',(-0.9,-2.02066721859313E-17,1.565));
#9905=CARTESIAN_POINT('Ctrl Pts',(-0.884745726183518,0.165,1.4));
#9906=CARTESIAN_POINT('Ctrl Pts',(-0.884745726183518,0.165,1.42076875940744));
#9907=CARTESIAN_POINT('Ctrl Pts',(-0.885552759505264,0.160839719007584,
1.44288889507334));
#9908=CARTESIAN_POINT('Ctrl Pts',(-0.888448648150043,0.14398647021669,1.48352706263377));
#9909=CARTESIAN_POINT('Ctrl Pts',(-0.890493604851638,0.131295993814186,
1.50204924397737));
#9910=CARTESIAN_POINT('Ctrl Pts',(-0.89431723432394,0.102049819008125,1.53129541878344));
#9911=CARTESIAN_POINT('Ctrl Pts',(-0.896347088899543,0.0835273920906824,
1.54398634598358));
#9912=CARTESIAN_POINT('Ctrl Pts',(-0.899208271860583,0.0428883760934128,
1.56083992183864));
#9913=CARTESIAN_POINT('Ctrl Pts',(-0.9,0.0207679427235068,1.565));
#9914=CARTESIAN_POINT('Ctrl Pts',(-0.9,2.77555756156289E-17,1.565));
#9915=CARTESIAN_POINT('',(-0.9,-8.63341285292134E-17,1.235));
#9916=CARTESIAN_POINT('Ctrl Pts',(-0.9,-6.24500451351651E-17,1.235));
#9917=CARTESIAN_POINT('Ctrl Pts',(-0.9,0.0207679427235068,1.235));
#9918=CARTESIAN_POINT('Ctrl Pts',(-0.899208271860583,0.0428883760934128,
1.23916007816136));
#9919=CARTESIAN_POINT('Ctrl Pts',(-0.896347088899543,0.0835273920906824,
1.25601365401642));
#9920=CARTESIAN_POINT('Ctrl Pts',(-0.89431723432394,0.102049819008125,1.26870458121656));
#9921=CARTESIAN_POINT('Ctrl Pts',(-0.890493604851638,0.131295993814186,
1.29795075602263));
#9922=CARTESIAN_POINT('Ctrl Pts',(-0.888448648150043,0.143986470216691,
1.31647293736623));
#9923=CARTESIAN_POINT('Ctrl Pts',(-0.885552759505264,0.160839719007584,
1.35711110492666));
#9924=CARTESIAN_POINT('Ctrl Pts',(-0.884745726183518,0.165,1.37923124059256));
#9925=CARTESIAN_POINT('Ctrl Pts',(-0.884745726183518,0.165,1.4));
#9926=CARTESIAN_POINT('Ctrl Pts',(-0.9,4.16333634234434E-17,1.565));
#9927=CARTESIAN_POINT('Ctrl Pts',(-0.9,-0.0207679427235068,1.565));
#9928=CARTESIAN_POINT('Ctrl Pts',(-0.899208271860583,-0.0428883760934127,
1.56083992183864));
#9929=CARTESIAN_POINT('Ctrl Pts',(-0.896347088899543,-0.0835273920906824,
1.54398634598358));
#9930=CARTESIAN_POINT('Ctrl Pts',(-0.89431723432394,-0.102049819008125,
1.53129541878344));
#9931=CARTESIAN_POINT('Ctrl Pts',(-0.890493604851638,-0.131295993814186,
1.50204924397737));
#9932=CARTESIAN_POINT('Ctrl Pts',(-0.888448648150043,-0.143986470216691,
1.48352706263377));
#9933=CARTESIAN_POINT('Ctrl Pts',(-0.885552759505264,-0.160839719007584,
1.44288889507334));
#9934=CARTESIAN_POINT('Ctrl Pts',(-0.884745726183518,-0.165,1.42076875940744));
#9935=CARTESIAN_POINT('Ctrl Pts',(-0.884745726183518,-0.165,1.37923124059256));
#9936=CARTESIAN_POINT('Ctrl Pts',(-0.885552759505264,-0.160839719007584,
1.35711110492666));
#9937=CARTESIAN_POINT('Ctrl Pts',(-0.888448648150043,-0.14398647021669,
1.31647293736623));
#9938=CARTESIAN_POINT('Ctrl Pts',(-0.890493604851638,-0.131295993814186,
1.29795075602263));
#9939=CARTESIAN_POINT('Ctrl Pts',(-0.89431723432394,-0.102049819008125,
1.26870458121656));
#9940=CARTESIAN_POINT('Ctrl Pts',(-0.896347088899543,-0.0835273920906825,
1.25601365401642));
#9941=CARTESIAN_POINT('Ctrl Pts',(-0.899208271860583,-0.0428883760934129,
1.23916007816136));
#9942=CARTESIAN_POINT('Ctrl Pts',(-0.9,-0.0207679427235069,1.235));
#9943=CARTESIAN_POINT('Ctrl Pts',(-0.9,-4.85722573273506E-17,1.235));
#9944=CARTESIAN_POINT('',(-0.505,-2.74505708527337E-17,1.565));
#9945=CARTESIAN_POINT('',(-1.,-2.02066721859313E-17,1.565));
#9946=CARTESIAN_POINT('',(-0.49,-0.122167917228706,1.51090536506409));
#9947=CARTESIAN_POINT('Ctrl Pts',(-0.49,-0.122167917228706,1.51090536506409));
#9948=CARTESIAN_POINT('Ctrl Pts',(-0.490448531679987,-0.120368913626296,
1.51288705930464));
#9949=CARTESIAN_POINT('Ctrl Pts',(-0.490895245371684,-0.118534896565231,
1.51481034122633));
#9950=CARTESIAN_POINT('Ctrl Pts',(-0.494795015531646,-0.102111993019358,
1.5312332447722));
#9951=CARTESIAN_POINT('Ctrl Pts',(-0.498442514607594,-0.0836597150224318,
1.54390845611142));
#9952=CARTESIAN_POINT('Ctrl Pts',(-0.50357781976106,-0.0430495960471595,
1.56079590960766));
#9953=CARTESIAN_POINT('Ctrl Pts',(-0.505,-0.020880094330741,1.565));
#9954=CARTESIAN_POINT('Ctrl Pts',(-0.505,0.,1.565));
#9955=CARTESIAN_POINT('',(-0.49,-0.122167917228706,1.28909463493591));
#9956=CARTESIAN_POINT('Origin',(-0.49,0.,1.4));
#9957=CARTESIAN_POINT('',(-0.505,-2.05139908226098E-17,1.235));
#9958=CARTESIAN_POINT('Ctrl Pts',(-0.505,2.77555756156289E-17,1.235));
#9959=CARTESIAN_POINT('Ctrl Pts',(-0.505,-0.020880094330741,1.235));
#9960=CARTESIAN_POINT('Ctrl Pts',(-0.50357781976106,-0.0430495960471594,
1.23920409039234));
#9961=CARTESIAN_POINT('Ctrl Pts',(-0.498442514607595,-0.0836597150224317,
1.25609154388858));
#9962=CARTESIAN_POINT('Ctrl Pts',(-0.494795015531646,-0.102111993019358,
1.2687667552278));
#9963=CARTESIAN_POINT('Ctrl Pts',(-0.490895245371684,-0.118534896565231,
1.28518965877367));
#9964=CARTESIAN_POINT('Ctrl Pts',(-0.490448531679987,-0.120368913626296,
1.28711294069536));
#9965=CARTESIAN_POINT('Ctrl Pts',(-0.49,-0.122167917228706,1.28909463493591));
#9966=CARTESIAN_POINT('Ctrl Pts',(-0.49,0.122167917228706,1.28909463493591));
#9967=CARTESIAN_POINT('Ctrl Pts',(-0.490448531679987,0.120368913626296,
1.28711294069536));
#9968=CARTESIAN_POINT('Ctrl Pts',(-0.490895245371684,0.118534896565231,
1.28518965877367));
#9969=CARTESIAN_POINT('Ctrl Pts',(-0.494795015531646,0.102111993019358,
1.2687667552278));
#9970=CARTESIAN_POINT('Ctrl Pts',(-0.498442514607594,0.0836597150224318,
1.25609154388858));
#9971=CARTESIAN_POINT('Ctrl Pts',(-0.50357781976106,0.0430495960471595,
1.23920409039234));
#9972=CARTESIAN_POINT('Ctrl Pts',(-0.505,0.020880094330741,1.235));
#9973=CARTESIAN_POINT('Ctrl Pts',(-0.505,-6.93889390390723E-18,1.235));
#9974=CARTESIAN_POINT('Ctrl Pts',(-0.505,-2.77555756156289E-17,1.565));
#9975=CARTESIAN_POINT('Ctrl Pts',(-0.505,0.020880094330741,1.565));
#9976=CARTESIAN_POINT('Ctrl Pts',(-0.50357781976106,0.0430495960471595,
1.56079590960766));
#9977=CARTESIAN_POINT('Ctrl Pts',(-0.498442514607594,0.0836597150224318,
1.54390845611142));
#9978=CARTESIAN_POINT('Ctrl Pts',(-0.494795015531646,0.102111993019358,
1.5312332447722));
#9979=CARTESIAN_POINT('Ctrl Pts',(-0.490895245371684,0.118534896565231,
1.51481034122633));
#9980=CARTESIAN_POINT('Ctrl Pts',(-0.490448531679987,0.120368913626296,
1.51288705930464));
#9981=CARTESIAN_POINT('Ctrl Pts',(-0.49,0.122167917228706,1.51090536506409));
#9982=CARTESIAN_POINT('Origin',(-0.49,0.,1.4));
#9983=CARTESIAN_POINT('',(-0.49,-0.122167917228706,1.));
#9984=CARTESIAN_POINT('Origin',(0.,0.,1.));
#9985=CARTESIAN_POINT('',(-0.505,-6.18446633569413E-17,1.8));
#9986=CARTESIAN_POINT('Origin',(0.,0.,1.8));
#9987=CARTESIAN_POINT('',(-0.505,-6.18446633569413E-17,1.));
#9988=CARTESIAN_POINT('',(-0.505,-6.18446633569413E-17,1.));
#9989=CARTESIAN_POINT('',(-0.505,-6.18446633569413E-17,1.));
#9990=CARTESIAN_POINT('Origin',(0.,0.,1.));
#9991=CARTESIAN_POINT('Origin',(0.,0.,1.));
#9992=CARTESIAN_POINT('',(-0.9,-1.10218211923262E-16,1.8));
#9993=CARTESIAN_POINT('Origin',(0.,0.,1.8));
#9994=CARTESIAN_POINT('',(-0.9,-1.10218211923262E-16,1.));
#9995=CARTESIAN_POINT('',(-0.9,-1.10218211923262E-16,1.));
#9996=CARTESIAN_POINT('',(-0.9,-1.10218211923262E-16,1.));
#9997=CARTESIAN_POINT('Origin',(0.,0.,1.));
#9998=CARTESIAN_POINT('Origin',(0.,0.,1.8));
#9999=CARTESIAN_POINT('Origin',(0.,0.,1.));
#10000=CARTESIAN_POINT('',(0.,0.,0.));
#10001=CARTESIAN_POINT('Origin',(3.,0.,5.6));
#10002=CARTESIAN_POINT('',(2.5,-6.12323399573677E-17,5.6));
#10003=CARTESIAN_POINT('Origin',(3.,0.,5.6));
#10004=CARTESIAN_POINT('',(2.7,-3.67394039744206E-17,5.6));
#10005=CARTESIAN_POINT('Origin',(3.,0.,5.6));
#10006=CARTESIAN_POINT('Origin',(3.,0.,5.2));
#10007=CARTESIAN_POINT('',(2.5,-6.12323399573677E-17,5.2));
#10008=CARTESIAN_POINT('Origin',(3.,0.,5.2));
#10009=CARTESIAN_POINT('',(2.7,3.67394039744206E-17,5.2));
#10010=CARTESIAN_POINT('Origin',(3.,0.,5.2));
#10011=CARTESIAN_POINT('Origin',(3.,0.,5.2));
#10012=CARTESIAN_POINT('',(2.5,-6.12323399573677E-17,5.2));
#10013=CARTESIAN_POINT('Origin',(3.,0.,4.8));
#10014=CARTESIAN_POINT('',(2.7,-3.67394039744206E-17,4.8));
#10015=CARTESIAN_POINT('',(2.7,-3.67394039744206E-17,4.8));
#10016=CARTESIAN_POINT('Origin',(3.,0.,4.8));
#10017=CARTESIAN_POINT('Origin',(3.,0.,4.8));
#10018=CARTESIAN_POINT('',(2.7,-3.67394039744206E-17,7.));
#10019=CARTESIAN_POINT('Origin',(3.,0.,7.));
#10020=CARTESIAN_POINT('',(2.7,-3.67394039744206E-17,4.8));
#10021=CARTESIAN_POINT('Origin',(3.,0.,7.));
#10022=CARTESIAN_POINT('Origin',(3.,0.,4.8));
#10023=CARTESIAN_POINT('',(0.,0.,0.));
#10024=CARTESIAN_POINT('Origin',(0.,0.,5.9));
#10025=CARTESIAN_POINT('',(-0.5,-6.12323399573677E-17,6.));
#10026=CARTESIAN_POINT('Origin',(0.,0.,6.));
#10027=CARTESIAN_POINT('',(-0.5,6.12323399573677E-17,6.8));
#10028=CARTESIAN_POINT('',(-0.5,-6.12323399573677E-17,5.9));
#10029=CARTESIAN_POINT('Origin',(0.,0.,6.8));
#10030=CARTESIAN_POINT('Origin',(0.,0.,6.));
#10031=CARTESIAN_POINT('',(0.,0.6,6.8));
#10032=CARTESIAN_POINT('',(0.,0.6,6.));
#10033=CARTESIAN_POINT('',(0.,0.6,6.));
#10034=CARTESIAN_POINT('',(0.,-0.6,6.8));
#10035=CARTESIAN_POINT('Origin',(0.,0.,6.8));
#10036=CARTESIAN_POINT('',(0.,-0.6,6.));
#10037=CARTESIAN_POINT('',(0.,-0.6,6.));
#10038=CARTESIAN_POINT('Origin',(0.,0.,6.));
#10039=CARTESIAN_POINT('Origin',(0.,0.,6.));
#10040=CARTESIAN_POINT('',(0.,-1.8,6.));
#10041=CARTESIAN_POINT('',(0.,0.95,6.));
#10042=CARTESIAN_POINT('',(0.,1.8,6.));
#10043=CARTESIAN_POINT('Origin',(0.,0.,6.));
#10044=CARTESIAN_POINT('',(0.,0.95,6.));
#10045=CARTESIAN_POINT('Origin',(0.,1.9,5.9));
#10046=CARTESIAN_POINT('',(0.,-1.8,6.8));
#10047=CARTESIAN_POINT('',(0.,0.95,6.8));
#10048=CARTESIAN_POINT('',(0.,-1.8,6.));
#10049=CARTESIAN_POINT('Origin',(0.,1.9,5.9));
#10050=CARTESIAN_POINT('',(0.,1.8,6.8));
#10051=CARTESIAN_POINT('',(0.,1.8,6.));
#10052=CARTESIAN_POINT('',(0.,0.95,6.8));
#10053=CARTESIAN_POINT('Origin',(0.,0.,6.));
#10054=CARTESIAN_POINT('Origin',(0.,0.,6.8));
#10055=CARTESIAN_POINT('Origin',(0.,0.,6.8));
#10056=CARTESIAN_POINT('',(0.,0.,0.));
#10057=CARTESIAN_POINT('Origin',(0.,0.,5.2));
#10058=CARTESIAN_POINT('',(-0.505,-6.18446633569413E-17,6.));
#10059=CARTESIAN_POINT('Origin',(0.,0.,6.));
#10060=CARTESIAN_POINT('',(-0.505,-6.18446633569413E-17,5.2));
#10061=CARTESIAN_POINT('',(-0.505,-6.18446633569413E-17,5.2));
#10062=CARTESIAN_POINT('Origin',(0.,0.,5.2));
#10063=CARTESIAN_POINT('Origin',(0.,0.,5.2));
#10064=CARTESIAN_POINT('',(-0.7,-8.57252759403147E-17,6.));
#10065=CARTESIAN_POINT('Origin',(0.,0.,6.));
#10066=CARTESIAN_POINT('',(-0.7,-8.57252759403147E-17,5.2));
#10067=CARTESIAN_POINT('',(-0.7,-8.57252759403147E-17,5.2));
#10068=CARTESIAN_POINT('Origin',(0.,0.,5.2));
#10069=CARTESIAN_POINT('Origin',(0.,0.,6.));
#10070=CARTESIAN_POINT('Origin',(0.,0.,5.2));
#10071=CARTESIAN_POINT('',(0.,0.,0.));
#10072=CARTESIAN_POINT('Origin',(0.,0.,6.8));
#10073=CARTESIAN_POINT('',(-0.225,-2.75545529808154E-17,7.));
#10074=CARTESIAN_POINT('Origin',(0.,0.,7.));
#10075=CARTESIAN_POINT('',(-0.225,-2.75545529808154E-17,6.8));
#10076=CARTESIAN_POINT('',(-0.225,-2.75545529808154E-17,6.8));
#10077=CARTESIAN_POINT('Origin',(0.,0.,6.8));
#10078=CARTESIAN_POINT('Origin',(0.,0.,6.8));
#10079=CARTESIAN_POINT('',(-0.7,-8.57252759403147E-17,7.));
#10080=CARTESIAN_POINT('Origin',(0.,0.,7.));
#10081=CARTESIAN_POINT('',(-0.7,-8.57252759403147E-17,6.8));
#10082=CARTESIAN_POINT('',(-0.7,-8.57252759403147E-17,6.8));
#10083=CARTESIAN_POINT('Origin',(0.,0.,6.8));
#10084=CARTESIAN_POINT('Origin',(0.,0.,7.));
#10085=CARTESIAN_POINT('Origin',(0.,0.,6.8));
#10086=CARTESIAN_POINT('',(0.,0.,0.));
#10087=CARTESIAN_POINT('Origin',(0.,0.,7.));
#10088=CARTESIAN_POINT('',(-0.4,-4.89858719658941E-17,8.5));
#10089=CARTESIAN_POINT('Origin',(0.,0.,8.5));
#10090=CARTESIAN_POINT('',(-0.4,-4.89858719658941E-17,7.));
#10091=CARTESIAN_POINT('',(-0.4,-4.89858719658941E-17,7.));
#10092=CARTESIAN_POINT('Origin',(0.,0.,7.));
#10093=CARTESIAN_POINT('Origin',(0.,0.,7.));
#10094=CARTESIAN_POINT('',(-1.4,-1.71450551880629E-16,8.5));
#10095=CARTESIAN_POINT('Origin',(0.,0.,8.5));
#10096=CARTESIAN_POINT('',(-1.4,-1.71450551880629E-16,7.));
#10097=CARTESIAN_POINT('',(-1.4,-1.71450551880629E-16,7.));
#10098=CARTESIAN_POINT('Origin',(0.,0.,7.));
#10099=CARTESIAN_POINT('Origin',(0.,0.,8.5));
#10100=CARTESIAN_POINT('Origin',(0.,0.,7.));
#10101=CARTESIAN_POINT('',(0.,0.,0.));
#10102=CARTESIAN_POINT('Origin',(0.0866025403784439,-0.4,-0.15));
#10103=CARTESIAN_POINT('',(0.173205080756888,-0.4,0.));
#10104=CARTESIAN_POINT('',(0.0866025403784439,-0.4,-0.15));
#10105=CARTESIAN_POINT('',(0.173205080756888,-0.4,0.));
#10106=CARTESIAN_POINT('',(0.0866025403784439,-0.64,-0.15));
#10107=CARTESIAN_POINT('',(0.0866025403784439,-0.4,-0.15));
#10108=CARTESIAN_POINT('',(0.173205080756888,-0.64,0.));
#10109=CARTESIAN_POINT('',(0.173205080756888,-0.64,0.));
#10110=CARTESIAN_POINT('',(0.173205080756888,-0.4,0.));
#10111=CARTESIAN_POINT('Origin',(-0.0866025403784438,-0.4,-0.15));
#10112=CARTESIAN_POINT('',(-0.0866025403784438,-0.4,-0.15));
#10113=CARTESIAN_POINT('',(0.0866025403784439,-0.4,-0.15));
#10114=CARTESIAN_POINT('',(-0.0866025403784438,-0.64,-0.15));
#10115=CARTESIAN_POINT('',(-0.0866025403784438,-0.4,-0.15));
#10116=CARTESIAN_POINT('',(0.0866025403784439,-0.64,-0.15));
#10117=CARTESIAN_POINT('Origin',(-0.173205080756888,-0.4,-2.77555756156289E-17));
#10118=CARTESIAN_POINT('',(-0.173205080756888,-0.4,-2.12115047744981E-17));
#10119=CARTESIAN_POINT('',(-0.0866025403784438,-0.4,-0.15));
#10120=CARTESIAN_POINT('',(-0.173205080756888,-0.64,-2.77555756156289E-17));
#10121=CARTESIAN_POINT('',(-0.173205080756888,-0.4,-2.12115047744981E-17));
#10122=CARTESIAN_POINT('',(-0.0866025403784438,-0.64,-0.15));
#10123=CARTESIAN_POINT('Origin',(-0.0866025403784439,-0.4,0.15));
#10124=CARTESIAN_POINT('',(-0.0866025403784439,-0.4,0.15));
#10125=CARTESIAN_POINT('',(-0.173205080756888,-0.4,-2.12115047744981E-17));
#10126=CARTESIAN_POINT('',(-0.0866025403784439,-0.64,0.15));
#10127=CARTESIAN_POINT('',(-0.0866025403784439,-0.4,0.15));
#10128=CARTESIAN_POINT('',(-0.173205080756888,-0.64,-2.12115047744981E-17));
#10129=CARTESIAN_POINT('Origin',(0.0866025403784439,-0.4,0.15));
#10130=CARTESIAN_POINT('',(0.0866025403784439,-0.4,0.15));
#10131=CARTESIAN_POINT('',(-0.0866025403784439,-0.4,0.15));
#10132=CARTESIAN_POINT('',(0.0866025403784439,-0.64,0.15));
#10133=CARTESIAN_POINT('',(0.0866025403784439,-0.4,0.15));
#10134=CARTESIAN_POINT('',(-0.0866025403784439,-0.64,0.15));
#10135=CARTESIAN_POINT('Origin',(0.173205080756888,-0.4,0.));
#10136=CARTESIAN_POINT('',(0.0866025403784439,-0.4,0.15));
#10137=CARTESIAN_POINT('',(0.0866025403784439,-0.64,0.15));
#10138=CARTESIAN_POINT('Origin',(0.,-0.4,-2.77555756156289E-17));
#10139=CARTESIAN_POINT('Origin',(0.,-0.64,-2.77555756156289E-17));
#10140=CARTESIAN_POINT('Origin',(0.,-1.,0.));
#10141=CARTESIAN_POINT('',(-0.1954,-1.,2.39295984553393E-17));
#10142=CARTESIAN_POINT('Origin',(0.,-1.,0.));
#10143=CARTESIAN_POINT('Origin',(0.3,0.4,0.));
#10144=CARTESIAN_POINT('',(-0.3,0.4,-3.67394039744206E-17));
#10145=CARTESIAN_POINT('Origin',(0.,0.4,0.));
#10146=CARTESIAN_POINT('Origin',(0.,0.375,0.));
#10147=CARTESIAN_POINT('',(-0.35,0.35,-4.28626379701573E-17));
#10148=CARTESIAN_POINT('Origin',(0.,0.35,0.));
#10149=CARTESIAN_POINT('',(-0.325,0.375,-3.9801020972289E-17));
#10150=CARTESIAN_POINT('Origin',(0.,0.19,0.));
#10151=CARTESIAN_POINT('',(-0.35,0.03,-4.28626379701574E-17));
#10152=CARTESIAN_POINT('Origin',(0.,0.03,0.));
#10153=CARTESIAN_POINT('',(-0.35,0.19,-4.28626379701574E-17));
#10154=CARTESIAN_POINT('Origin',(0.,0.0149999999999999,0.));
#10155=CARTESIAN_POINT('',(-0.32,-3.29597460435593E-17,-3.91886975727153E-17));
#10156=CARTESIAN_POINT('Origin',(0.,0.,0.));
#10157=CARTESIAN_POINT('',(-0.335,0.0149999999999999,-4.10256677714363E-17));
#10158=CARTESIAN_POINT('Origin',(0.22,0.,0.));
#10159=CARTESIAN_POINT('',(-0.22,-6.93889390390723E-18,-2.69422295812418E-17));
#10160=CARTESIAN_POINT('Origin',(0.,0.,0.));
#10161=CARTESIAN_POINT('Origin',(0.,-0.02,0.));
#10162=CARTESIAN_POINT('',(-0.1954,-0.0492,2.39295984553393E-17));
#10163=CARTESIAN_POINT('Origin',(0.,-0.0492,0.));
#10164=CARTESIAN_POINT('',(-0.21,-0.02,-2.57175827820944E-17));
#10165=CARTESIAN_POINT('Origin',(0.,-0.8,0.));
#10166=CARTESIAN_POINT('',(-0.1954,-0.8,-2.39295984553393E-17));
#10167=CARTESIAN_POINT('',(0.,0.,0.));
#10168=CARTESIAN_POINT('',(0.,0.,0.));
#10169=CARTESIAN_POINT('',(0.,0.,0.));
#10170=CARTESIAN_POINT('',(0.,0.,0.));
#10171=CARTESIAN_POINT('',(0.,0.,0.));
#10172=CARTESIAN_POINT('',(-1.7,-1.7,2.2));
#10173=CARTESIAN_POINT('',(-1.7,1.7,2.2));
#10174=CARTESIAN_POINT('',(5.94264068711928,-1.7,2.2));
#10175=CARTESIAN_POINT('',(5.94264068711928,1.7,2.2));
#10176=CARTESIAN_POINT('',(0.,0.,2.5));
#10177=CARTESIAN_POINT('',(1.72,0.,4.));
#10178=CARTESIAN_POINT('',(0.,1.72,4.));
#10179=CARTESIAN_POINT('',(-1.72,2.10639249453345E-16,4.));
#10180=CARTESIAN_POINT('',(-2.22044604925031E-16,-1.72,4.));
#10181=CARTESIAN_POINT('',(4.24264068711929,0.,2.5));
#10182=CARTESIAN_POINT('',(5.96264068711929,0.,4.));
#10183=CARTESIAN_POINT('',(4.24264068711929,1.72,4.));
#10184=CARTESIAN_POINT('',(2.52264068711929,2.10639249453345E-16,4.));
#10185=CARTESIAN_POINT('',(4.24264068711929,-1.72,4.));
#10186=CARTESIAN_POINT('',(0.,0.,0.));
#10187=CARTESIAN_POINT('',(0.,0.,0.));
#10188=CARTESIAN_POINT('Origin',(2.9698484809835,-1.27279220613579,5.9));
#10189=CARTESIAN_POINT('',(2.8048484809835,-1.27279220613579,6.));
#10190=CARTESIAN_POINT('Origin',(2.9698484809835,-1.27279220613579,6.));
#10191=CARTESIAN_POINT('',(2.8048484809835,-1.27279220613579,6.8));
#10192=CARTESIAN_POINT('',(2.8048484809835,-1.27279220613579,5.9));
#10193=CARTESIAN_POINT('Origin',(2.9698484809835,-1.27279220613579,6.8));
#10194=CARTESIAN_POINT('Origin',(2.9698484809835,1.27279220613579,5.9));
#10195=CARTESIAN_POINT('',(2.8048484809835,1.27279220613579,6.));
#10196=CARTESIAN_POINT('Origin',(2.9698484809835,1.27279220613579,6.));
#10197=CARTESIAN_POINT('',(2.8048484809835,1.27279220613579,6.8));
#10198=CARTESIAN_POINT('',(2.8048484809835,1.27279220613579,5.9));
#10199=CARTESIAN_POINT('Origin',(2.9698484809835,1.27279220613579,6.8));
#10200=CARTESIAN_POINT('Origin',(5.51543289325507,1.27279220613579,5.9));
#10201=CARTESIAN_POINT('',(5.35043289325507,1.27279220613579,6.));
#10202=CARTESIAN_POINT('Origin',(5.51543289325507,1.27279220613579,6.));
#10203=CARTESIAN_POINT('',(5.35043289325507,1.27279220613579,6.8));
#10204=CARTESIAN_POINT('',(5.35043289325507,1.27279220613579,5.9));
#10205=CARTESIAN_POINT('Origin',(5.51543289325507,1.27279220613579,6.8));
#10206=CARTESIAN_POINT('Origin',(5.51543289325507,-1.27279220613579,5.9));
#10207=CARTESIAN_POINT('',(5.35043289325507,-1.27279220613579,6.));
#10208=CARTESIAN_POINT('Origin',(5.51543289325507,-1.27279220613579,6.));
#10209=CARTESIAN_POINT('',(5.35043289325507,-1.27279220613579,6.8));
#10210=CARTESIAN_POINT('',(5.35043289325507,-1.27279220613579,5.9));
#10211=CARTESIAN_POINT('Origin',(5.51543289325507,-1.27279220613579,6.8));
#10212=CARTESIAN_POINT('Origin',(1.24264068711928,-3.,5.9));
#10213=CARTESIAN_POINT('',(3.04549806673909,-2.75079071295314,6.));
#10214=CARTESIAN_POINT('',(1.49184997416615,-1.19714262038019,6.));
#10215=CARTESIAN_POINT('Origin',(1.24264068711928,-3.,6.));
#10216=CARTESIAN_POINT('',(3.04549806673909,-2.75079071295314,6.8));
#10217=CARTESIAN_POINT('',(3.04549806673909,-2.75079071295314,5.9));
#10218=CARTESIAN_POINT('',(1.49184997416615,-1.19714262038019,6.8));
#10219=CARTESIAN_POINT('Origin',(1.24264068711928,-3.,6.8));
#10220=CARTESIAN_POINT('',(1.49184997416615,-1.19714262038019,5.9));
#10221=CARTESIAN_POINT('Origin',(1.24264068711929,3.,5.9));
#10222=CARTESIAN_POINT('',(1.49184997416615,1.19714262038019,6.));
#10223=CARTESIAN_POINT('',(3.04549806673909,2.75079071295314,6.));
#10224=CARTESIAN_POINT('Origin',(1.24264068711929,3.,6.));
#10225=CARTESIAN_POINT('',(1.49184997416615,1.19714262038019,6.8));
#10226=CARTESIAN_POINT('',(1.49184997416615,1.19714262038019,5.9));
#10227=CARTESIAN_POINT('',(3.04549806673909,2.75079071295314,6.8));
#10228=CARTESIAN_POINT('Origin',(1.24264068711929,3.,6.8));
#10229=CARTESIAN_POINT('',(3.04549806673909,2.75079071295314,5.9));
#10230=CARTESIAN_POINT('Origin',(7.24264068711929,3.,5.9));
#10231=CARTESIAN_POINT('',(5.43978330749948,2.75079071295314,6.));
#10232=CARTESIAN_POINT('',(6.99343140007243,1.19714262038019,6.));
#10233=CARTESIAN_POINT('Origin',(7.24264068711929,3.,6.));
#10234=CARTESIAN_POINT('',(5.43978330749948,2.75079071295314,6.8));
#10235=CARTESIAN_POINT('',(5.43978330749948,2.75079071295314,5.9));
#10236=CARTESIAN_POINT('',(6.99343140007243,1.19714262038019,6.8));
#10237=CARTESIAN_POINT('Origin',(7.24264068711929,3.,6.8));
#10238=CARTESIAN_POINT('',(6.99343140007243,1.19714262038019,5.9));
#10239=CARTESIAN_POINT('Origin',(7.24264068711929,-3.,5.9));
#10240=CARTESIAN_POINT('',(6.99343140007242,-1.19714262038019,6.8));
#10241=CARTESIAN_POINT('',(6.99343140007242,-1.19714262038019,6.));
#10242=CARTESIAN_POINT('',(6.99343140007243,-1.19714262038019,5.9));
#10243=CARTESIAN_POINT('',(5.43978330749948,-2.75079071295314,6.8));
#10244=CARTESIAN_POINT('Origin',(7.24264068711929,-3.,6.8));
#10245=CARTESIAN_POINT('',(5.43978330749948,-2.75079071295314,6.));
#10246=CARTESIAN_POINT('',(5.43978330749948,-2.75079071295314,5.9));
#10247=CARTESIAN_POINT('Origin',(7.24264068711929,-3.,6.));
#10248=CARTESIAN_POINT('Origin',(4.24264068711929,0.,6.));
#10249=CARTESIAN_POINT('',(3.81264068711929,-2.96902340846279,6.));
#10250=CARTESIAN_POINT('Origin',(4.24264068711929,0.,6.));
#10251=CARTESIAN_POINT('',(3.81264068711929,-2.96902340846279,6.8));
#10252=CARTESIAN_POINT('',(3.81264068711929,-2.96902340846279,6.));
#10253=CARTESIAN_POINT('Origin',(4.24264068711929,0.,6.8));
#10254=CARTESIAN_POINT('Origin',(4.24264068711929,0.,6.));
#10255=CARTESIAN_POINT('',(1.2736172786565,0.43,6.));
#10256=CARTESIAN_POINT('Origin',(4.24264068711929,0.,6.));
#10257=CARTESIAN_POINT('',(1.2736172786565,0.43,6.8));
#10258=CARTESIAN_POINT('',(1.2736172786565,0.43,6.));
#10259=CARTESIAN_POINT('Origin',(4.24264068711929,0.,6.8));
#10260=CARTESIAN_POINT('Origin',(4.24264068711929,0.,6.));
#10261=CARTESIAN_POINT('',(4.67264068711929,2.96902340846279,6.));
#10262=CARTESIAN_POINT('Origin',(4.24264068711929,0.,6.));
#10263=CARTESIAN_POINT('',(4.67264068711929,2.96902340846279,6.8));
#10264=CARTESIAN_POINT('',(4.67264068711929,2.96902340846279,6.));
#10265=CARTESIAN_POINT('Origin',(4.24264068711929,0.,6.8));
#10266=CARTESIAN_POINT('Origin',(4.24264068711929,0.,6.8));
#10267=CARTESIAN_POINT('',(3.81264068711929,-2.6,6.8));
#10268=CARTESIAN_POINT('',(3.81264068711929,-1.3,6.8));
#10269=CARTESIAN_POINT('',(3.92264068711928,-2.6,6.8));
#10270=CARTESIAN_POINT('',(4.45764068711929,-2.6,6.8));
#10271=CARTESIAN_POINT('',(3.92264068711928,-1.,6.8));
#10272=CARTESIAN_POINT('',(3.92264068711929,-0.5,6.8));
#10273=CARTESIAN_POINT('',(4.56264068711929,-1.,6.8));
#10274=CARTESIAN_POINT('Origin',(4.24264068711929,-1.,6.8));
#10275=CARTESIAN_POINT('',(4.56264068711929,-2.6,6.8));
#10276=CARTESIAN_POINT('',(4.56264068711929,-1.8,6.8));
#10277=CARTESIAN_POINT('',(4.67264068711928,-2.6,6.8));
#10278=CARTESIAN_POINT('',(4.45764068711929,-2.6,6.8));
#10279=CARTESIAN_POINT('',(4.67264068711928,-2.96902340846279,6.8));
#10280=CARTESIAN_POINT('',(4.67264068711929,-1.8,6.8));
#10281=CARTESIAN_POINT('Origin',(4.24264068711929,0.,6.8));
#10282=CARTESIAN_POINT('',(7.21166409558207,-0.43,6.8));
#10283=CARTESIAN_POINT('Origin',(4.24264068711929,0.,6.8));
#10284=CARTESIAN_POINT('',(6.84264068711929,-0.43,6.8));
#10285=CARTESIAN_POINT('',(5.54264068711929,-0.43,6.8));
#10286=CARTESIAN_POINT('',(6.84264068711929,-0.32,6.8));
#10287=CARTESIAN_POINT('',(6.84264068711929,0.215,6.8));
#10288=CARTESIAN_POINT('',(5.24264068711929,-0.32,6.8));
#10289=CARTESIAN_POINT('',(4.74264068711929,-0.32,6.8));
#10290=CARTESIAN_POINT('',(5.24264068711929,0.32,6.8));
#10291=CARTESIAN_POINT('Origin',(5.24264068711929,0.,6.8));
#10292=CARTESIAN_POINT('',(6.84264068711929,0.32,6.8));
#10293=CARTESIAN_POINT('',(6.04264068711929,0.32,6.8));
#10294=CARTESIAN_POINT('',(6.84264068711929,0.43,6.8));
#10295=CARTESIAN_POINT('',(6.84264068711929,0.215,6.8));
#10296=CARTESIAN_POINT('',(7.21166409558207,0.43,6.8));
#10297=CARTESIAN_POINT('',(6.04264068711929,0.43,6.8));
#10298=CARTESIAN_POINT('Origin',(4.24264068711929,0.,6.8));
#10299=CARTESIAN_POINT('',(4.67264068711929,2.6,6.8));
#10300=CARTESIAN_POINT('',(4.67264068711929,1.3,6.8));
#10301=CARTESIAN_POINT('',(4.56264068711929,2.6,6.8));
#10302=CARTESIAN_POINT('',(4.02764068711929,2.6,6.8));
#10303=CARTESIAN_POINT('',(4.56264068711929,1.,6.8));
#10304=CARTESIAN_POINT('',(4.56264068711929,0.5,6.8));
#10305=CARTESIAN_POINT('',(3.92264068711928,1.,6.8));
#10306=CARTESIAN_POINT('Origin',(4.24264068711929,1.,6.8));
#10307=CARTESIAN_POINT('',(3.92264068711929,2.6,6.8));
#10308=CARTESIAN_POINT('',(3.92264068711929,1.8,6.8));
#10309=CARTESIAN_POINT('',(3.81264068711929,2.6,6.8));
#10310=CARTESIAN_POINT('',(4.02764068711929,2.6,6.8));
#10311=CARTESIAN_POINT('',(3.81264068711929,2.96902340846279,6.8));
#10312=CARTESIAN_POINT('',(3.81264068711929,1.8,6.8));
#10313=CARTESIAN_POINT('Origin',(4.24264068711929,0.,6.8));
#10314=CARTESIAN_POINT('',(1.64264068711929,0.43,6.8));
#10315=CARTESIAN_POINT('',(2.94264068711929,0.43,6.8));
#10316=CARTESIAN_POINT('',(1.64264068711929,0.32,6.8));
#10317=CARTESIAN_POINT('',(1.64264068711929,-0.215,6.8));
#10318=CARTESIAN_POINT('',(3.24264068711929,0.32,6.8));
#10319=CARTESIAN_POINT('',(3.74264068711929,0.32,6.8));
#10320=CARTESIAN_POINT('',(3.24264068711929,-0.32,6.8));
#10321=CARTESIAN_POINT('Origin',(3.24264068711929,1.22464679914735E-16,
6.8));
#10322=CARTESIAN_POINT('',(1.64264068711929,-0.32,6.8));
#10323=CARTESIAN_POINT('',(2.44264068711929,-0.32,6.8));
#10324=CARTESIAN_POINT('',(1.64264068711929,-0.43,6.8));
#10325=CARTESIAN_POINT('',(1.64264068711929,-0.215,6.8));
#10326=CARTESIAN_POINT('',(1.2736172786565,-0.43,6.8));
#10327=CARTESIAN_POINT('',(2.44264068711929,-0.43,6.8));
#10328=CARTESIAN_POINT('Origin',(4.24264068711929,0.,6.8));
#10329=CARTESIAN_POINT('Origin',(4.24264068711929,0.,6.));
#10330=CARTESIAN_POINT('',(7.21166409558207,-0.43,6.));
#10331=CARTESIAN_POINT('Origin',(4.24264068711929,0.,6.));
#10332=CARTESIAN_POINT('',(7.21166409558207,-0.43,6.));
#10333=CARTESIAN_POINT('Origin',(4.24264068711929,0.,6.));
#10334=CARTESIAN_POINT('',(4.67264068711928,-2.96902340846279,6.));
#10335=CARTESIAN_POINT('',(4.67264068711928,-2.96902340846279,6.));
#10336=CARTESIAN_POINT('Origin',(4.24264068711929,0.,6.));
#10337=CARTESIAN_POINT('Origin',(4.67264068711928,-3.6,5.9));
#10338=CARTESIAN_POINT('',(4.67264068711928,-2.6,6.));
#10339=CARTESIAN_POINT('',(4.67264068711928,-2.6,5.9));
#10340=CARTESIAN_POINT('',(4.67264068711929,-1.8,6.));
#10341=CARTESIAN_POINT('Origin',(4.67264068711928,-2.6,5.9));
#10342=CARTESIAN_POINT('',(4.56264068711929,-2.6,6.));
#10343=CARTESIAN_POINT('',(4.56264068711929,-2.6,5.9));
#10344=CARTESIAN_POINT('',(4.45764068711929,-2.6,6.));
#10345=CARTESIAN_POINT('Origin',(4.67264068711928,-2.6,5.9));
#10346=CARTESIAN_POINT('',(3.81264068711929,-2.6,6.));
#10347=CARTESIAN_POINT('',(3.81264068711929,-2.6,5.9));
#10348=CARTESIAN_POINT('',(3.92264068711928,-2.6,6.));
#10349=CARTESIAN_POINT('',(4.45764068711929,-2.6,6.));
#10350=CARTESIAN_POINT('',(3.92264068711928,-2.6,5.9));
#10351=CARTESIAN_POINT('Origin',(3.81264068711929,-2.6,5.9));
#10352=CARTESIAN_POINT('',(3.81264068711929,-1.3,6.));
#10353=CARTESIAN_POINT('Origin',(3.92264068711928,-1.,5.9));
#10354=CARTESIAN_POINT('',(3.92264068711928,-1.,6.));
#10355=CARTESIAN_POINT('',(3.92264068711929,-0.5,6.));
#10356=CARTESIAN_POINT('',(3.92264068711928,-1.,5.9));
#10357=CARTESIAN_POINT('Origin',(4.24264068711929,0.,6.));
#10358=CARTESIAN_POINT('',(1.2736172786565,-0.43,6.));
#10359=CARTESIAN_POINT('Origin',(4.24264068711929,0.,6.));
#10360=CARTESIAN_POINT('',(1.64264068711929,-0.43,6.));
#10361=CARTESIAN_POINT('',(2.44264068711929,-0.43,6.));
#10362=CARTESIAN_POINT('',(1.64264068711929,-0.32,6.));
#10363=CARTESIAN_POINT('',(1.64264068711929,-0.215,6.));
#10364=CARTESIAN_POINT('',(3.24264068711929,-0.32,6.));
#10365=CARTESIAN_POINT('',(2.44264068711929,-0.32,6.));
#10366=CARTESIAN_POINT('',(3.54884068711929,-0.0929599913941466,6.));
#10367=CARTESIAN_POINT('Origin',(3.24264068711929,1.22464679914735E-16,
6.));
#10368=CARTESIAN_POINT('',(4.14968069572514,-0.6938,6.));
#10369=CARTESIAN_POINT('Origin',(4.24264068711929,0.,6.));
#10370=CARTESIAN_POINT('Origin',(4.24264068711929,-1.,6.));
#10371=CARTESIAN_POINT('Origin',(4.24264068711929,0.,6.));
#10372=CARTESIAN_POINT('',(4.56264068711929,-1.,6.));
#10373=CARTESIAN_POINT('',(4.56264068711929,-1.8,6.));
#10374=CARTESIAN_POINT('',(4.33560067851344,-0.6938,6.));
#10375=CARTESIAN_POINT('Origin',(4.24264068711929,-1.,6.));
#10376=CARTESIAN_POINT('',(4.93644068711929,-0.0929599913941494,6.));
#10377=CARTESIAN_POINT('Origin',(4.24264068711929,0.,6.));
#10378=CARTESIAN_POINT('',(5.24264068711929,-0.32,6.));
#10379=CARTESIAN_POINT('Origin',(5.24264068711929,0.,6.));
#10380=CARTESIAN_POINT('',(6.84264068711929,-0.32,6.));
#10381=CARTESIAN_POINT('',(4.74264068711929,-0.32,6.));
#10382=CARTESIAN_POINT('',(6.84264068711929,-0.43,6.));
#10383=CARTESIAN_POINT('',(6.84264068711929,0.215,6.));
#10384=CARTESIAN_POINT('',(5.54264068711929,-0.43,6.));
#10385=CARTESIAN_POINT('Origin',(4.24264068711929,-1.,5.9));
#10386=CARTESIAN_POINT('',(4.33560067851343,-0.6938,5.9));
#10387=CARTESIAN_POINT('',(4.14968069572514,-0.6938,5.9));
#10388=CARTESIAN_POINT('Origin',(4.24264068711929,0.,5.9));
#10389=CARTESIAN_POINT('Origin',(4.24264068711929,-1.,5.9));
#10390=CARTESIAN_POINT('Origin',(4.24264068711929,-1.,5.9));
#10391=CARTESIAN_POINT('',(4.33560067851343,-0.6938,5.9));
#10392=CARTESIAN_POINT('',(4.56264068711929,-1.,5.9));
#10393=CARTESIAN_POINT('',(4.14968069572514,-0.6938,5.9));
#10394=CARTESIAN_POINT('Origin',(4.24264068711929,0.,2.95));
#10395=CARTESIAN_POINT('',(3.54884068711929,-0.0929599913941465,5.9));
#10396=CARTESIAN_POINT('',(3.54884068711929,-0.0929599913941465,5.9));
#10397=CARTESIAN_POINT('',(3.54264068711929,-8.57252759403147E-17,5.9));
#10398=CARTESIAN_POINT('Origin',(4.24264068711929,0.,5.9));
#10399=CARTESIAN_POINT('',(3.54264068711929,-8.57252759403147E-17,2.95));
#10400=CARTESIAN_POINT('',(3.54264068711929,-8.57252759403147E-17,2.95));
#10401=CARTESIAN_POINT('Origin',(4.24264068711929,0.,2.95));
#10402=CARTESIAN_POINT('',(3.54884068711929,0.0929599913941467,5.9));
#10403=CARTESIAN_POINT('Origin',(4.24264068711929,0.,5.9));
#10404=CARTESIAN_POINT('',(3.54884068711929,0.0929599913941468,6.));
#10405=CARTESIAN_POINT('',(3.54884068711929,0.0929599913941467,5.9));
#10406=CARTESIAN_POINT('',(4.14968069572514,0.6938,6.));
#10407=CARTESIAN_POINT('Origin',(4.24264068711929,0.,6.));
#10408=CARTESIAN_POINT('',(4.14968069572514,0.6938,5.9));
#10409=CARTESIAN_POINT('',(4.14968069572514,0.6938,5.9));
#10410=CARTESIAN_POINT('',(4.33560067851343,0.6938,5.9));
#10411=CARTESIAN_POINT('Origin',(4.24264068711929,0.,5.9));
#10412=CARTESIAN_POINT('',(4.33560067851344,0.6938,6.));
#10413=CARTESIAN_POINT('',(4.33560067851343,0.6938,5.9));
#10414=CARTESIAN_POINT('',(4.93644068711929,0.0929599913941494,6.));
#10415=CARTESIAN_POINT('Origin',(4.24264068711929,0.,6.));
#10416=CARTESIAN_POINT('',(4.93644068711929,0.0929599913941487,5.9));
#10417=CARTESIAN_POINT('',(4.93644068711929,0.0929599913941487,5.9));
#10418=CARTESIAN_POINT('',(4.93644068711929,-0.0929599913941487,5.9));
#10419=CARTESIAN_POINT('Origin',(4.24264068711929,0.,5.9));
#10420=CARTESIAN_POINT('',(4.93644068711929,-0.0929599913941487,5.9));
#10421=CARTESIAN_POINT('Origin',(4.56264068711929,-3.6,5.9));
#10422=CARTESIAN_POINT('Origin',(4.24264068711929,0.,6.));
#10423=CARTESIAN_POINT('',(1.2736172786565,-0.43,6.));
#10424=CARTESIAN_POINT('Origin',(0.642640687119285,-0.43,5.9));
#10425=CARTESIAN_POINT('',(1.64264068711929,-0.43,5.9));
#10426=CARTESIAN_POINT('Origin',(1.64264068711929,-0.43,5.9));
#10427=CARTESIAN_POINT('',(1.64264068711929,-0.32,5.9));
#10428=CARTESIAN_POINT('Origin',(1.64264068711929,-0.43,5.9));
#10429=CARTESIAN_POINT('',(1.64264068711929,0.43,6.));
#10430=CARTESIAN_POINT('',(1.64264068711929,0.43,5.9));
#10431=CARTESIAN_POINT('',(1.64264068711929,0.32,6.));
#10432=CARTESIAN_POINT('',(1.64264068711929,-0.215,6.));
#10433=CARTESIAN_POINT('',(1.64264068711929,0.32,5.9));
#10434=CARTESIAN_POINT('Origin',(1.64264068711929,0.43,5.9));
#10435=CARTESIAN_POINT('',(2.94264068711929,0.43,6.));
#10436=CARTESIAN_POINT('Origin',(3.24264068711929,0.32,5.9));
#10437=CARTESIAN_POINT('',(3.24264068711929,0.32,6.));
#10438=CARTESIAN_POINT('',(3.74264068711929,0.32,6.));
#10439=CARTESIAN_POINT('',(3.24264068711929,0.32,5.9));
#10440=CARTESIAN_POINT('Origin',(4.24264068711929,0.,6.));
#10441=CARTESIAN_POINT('',(3.81264068711929,2.96902340846279,6.));
#10442=CARTESIAN_POINT('Origin',(4.24264068711929,0.,6.));
#10443=CARTESIAN_POINT('',(3.81264068711929,2.6,6.));
#10444=CARTESIAN_POINT('',(3.81264068711929,1.8,6.));
#10445=CARTESIAN_POINT('',(3.92264068711929,2.6,6.));
#10446=CARTESIAN_POINT('',(4.02764068711929,2.6,6.));
#10447=CARTESIAN_POINT('',(3.92264068711928,1.,6.));
#10448=CARTESIAN_POINT('',(3.92264068711929,1.8,6.));
#10449=CARTESIAN_POINT('Origin',(4.24264068711929,1.,6.));
#10450=CARTESIAN_POINT('Origin',(3.24264068711929,1.22464679914735E-16,
6.));
#10451=CARTESIAN_POINT('Origin',(3.24264068711929,1.11022302462516E-16,
5.9));
#10452=CARTESIAN_POINT('Origin',(3.24264068711929,1.22464679914735E-16,
5.9));
#10453=CARTESIAN_POINT('Origin',(3.24264068711929,1.22464679914735E-16,
5.9));
#10454=CARTESIAN_POINT('',(3.24264068711929,-0.32,5.9));
#10455=CARTESIAN_POINT('Origin',(0.642640687119285,-0.32,5.9));
#10456=CARTESIAN_POINT('Origin',(4.24264068711929,0.,6.));
#10457=CARTESIAN_POINT('',(3.81264068711929,2.96902340846279,6.));
#10458=CARTESIAN_POINT('Origin',(3.81264068711929,3.6,5.9));
#10459=CARTESIAN_POINT('',(3.81264068711929,2.6,5.9));
#10460=CARTESIAN_POINT('Origin',(3.81264068711929,2.6,5.9));
#10461=CARTESIAN_POINT('',(3.92264068711928,2.6,5.9));
#10462=CARTESIAN_POINT('Origin',(3.81264068711929,2.6,5.9));
#10463=CARTESIAN_POINT('',(4.67264068711929,2.6,6.));
#10464=CARTESIAN_POINT('',(4.67264068711929,2.6,5.9));
#10465=CARTESIAN_POINT('',(4.56264068711929,2.6,6.));
#10466=CARTESIAN_POINT('',(4.02764068711929,2.6,6.));
#10467=CARTESIAN_POINT('',(4.56264068711929,2.6,5.9));
#10468=CARTESIAN_POINT('Origin',(4.67264068711929,2.6,5.9));
#10469=CARTESIAN_POINT('',(4.67264068711929,1.3,6.));
#10470=CARTESIAN_POINT('Origin',(4.56264068711929,1.,5.9));
#10471=CARTESIAN_POINT('',(4.56264068711929,1.,6.));
#10472=CARTESIAN_POINT('',(4.56264068711929,0.5,6.));
#10473=CARTESIAN_POINT('',(4.56264068711929,1.,5.9));
#10474=CARTESIAN_POINT('Origin',(4.24264068711929,0.,6.));
#10475=CARTESIAN_POINT('',(7.21166409558207,0.43,6.));
#10476=CARTESIAN_POINT('Origin',(4.24264068711929,0.,6.));
#10477=CARTESIAN_POINT('',(6.84264068711929,0.43,6.));
#10478=CARTESIAN_POINT('',(6.04264068711929,0.43,6.));
#10479=CARTESIAN_POINT('',(6.84264068711929,0.32,6.));
#10480=CARTESIAN_POINT('',(6.84264068711929,0.215,6.));
#10481=CARTESIAN_POINT('',(5.24264068711929,0.32,6.));
#10482=CARTESIAN_POINT('',(6.04264068711929,0.32,6.));
#10483=CARTESIAN_POINT('Origin',(5.24264068711929,0.,6.));
#10484=CARTESIAN_POINT('Origin',(4.24264068711929,1.,6.));
#10485=CARTESIAN_POINT('Origin',(4.24264068711929,1.,5.9));
#10486=CARTESIAN_POINT('Origin',(4.24264068711929,1.,5.9));
#10487=CARTESIAN_POINT('Origin',(4.24264068711929,1.,5.9));
#10488=CARTESIAN_POINT('',(3.92264068711928,1.,5.9));
#10489=CARTESIAN_POINT('Origin',(3.92264068711928,3.6,5.9));
#10490=CARTESIAN_POINT('Origin',(4.24264068711929,0.,6.));
#10491=CARTESIAN_POINT('',(7.21166409558207,0.43,6.));
#10492=CARTESIAN_POINT('Origin',(7.84264068711929,0.43,5.9));
#10493=CARTESIAN_POINT('',(6.84264068711929,0.43,5.9));
#10494=CARTESIAN_POINT('Origin',(6.84264068711929,-0.43,5.9));
#10495=CARTESIAN_POINT('',(6.84264068711929,-0.43,5.9));
#10496=CARTESIAN_POINT('Origin',(6.84264068711929,0.43,5.9));
#10497=CARTESIAN_POINT('',(6.84264068711929,-0.32,5.9));
#10498=CARTESIAN_POINT('Origin',(6.84264068711929,0.43,5.9));
#10499=CARTESIAN_POINT('',(6.84264068711929,0.32,5.9));
#10500=CARTESIAN_POINT('Origin',(5.24264068711929,0.,5.9));
#10501=CARTESIAN_POINT('Origin',(5.24264068711929,0.,5.9));
#10502=CARTESIAN_POINT('Origin',(5.24264068711929,0.,5.9));
#10503=CARTESIAN_POINT('',(5.24264068711929,0.32,5.9));
#10504=CARTESIAN_POINT('',(5.24264068711929,-0.32,5.9));
#10505=CARTESIAN_POINT('Origin',(7.84264068711929,0.32,5.9));
#10506=CARTESIAN_POINT('Origin',(5.24264068711929,-0.32,5.9));
#10507=CARTESIAN_POINT('Origin',(4.24264068711929,0.,2.95));
#10508=CARTESIAN_POINT('',(3.74264068711929,6.12323399573677E-17,2.95));
#10509=CARTESIAN_POINT('Origin',(4.24264068711929,0.,2.95));
#10510=CARTESIAN_POINT('Origin',(4.24264068711929,0.,1.));
#10511=CARTESIAN_POINT('',(3.74264068711929,-6.12323399573677E-17,1.));
#10512=CARTESIAN_POINT('',(3.74264068711929,-6.12323399573677E-17,1.));
#10513=CARTESIAN_POINT('Origin',(4.24264068711929,0.,1.));
#10514=CARTESIAN_POINT('Origin',(4.24264068711929,0.,1.));
#10515=CARTESIAN_POINT('',(0.,0.,0.));
#10516=CARTESIAN_POINT('Origin',(4.24264068711929,0.,1.8));
#10517=CARTESIAN_POINT('',(3.73764068711929,-6.18446633569413E-17,2.05));
#10518=CARTESIAN_POINT('Origin',(4.24264068711929,0.,2.05));
#10519=CARTESIAN_POINT('',(3.73764068711929,-6.18446633569413E-17,1.8));
#10520=CARTESIAN_POINT('',(3.73764068711929,-6.18446633569413E-17,1.8));
#10521=CARTESIAN_POINT('Origin',(4.24264068711929,0.,1.8));
#10522=CARTESIAN_POINT('Origin',(4.24264068711929,0.,1.8));
#10523=CARTESIAN_POINT('',(3.54264068711929,-8.57252759403147E-17,2.05));
#10524=CARTESIAN_POINT('Origin',(4.24264068711929,0.,2.05));
#10525=CARTESIAN_POINT('',(3.54264068711929,-8.57252759403147E-17,1.8));
#10526=CARTESIAN_POINT('',(3.54264068711929,-8.57252759403147E-17,1.8));
#10527=CARTESIAN_POINT('Origin',(4.24264068711929,0.,1.8));
#10528=CARTESIAN_POINT('Origin',(4.24264068711929,0.,2.05));
#10529=CARTESIAN_POINT('Origin',(4.24264068711929,0.,1.8));
#10530=CARTESIAN_POINT('',(0.,0.,0.));
#10531=CARTESIAN_POINT('Origin',(4.24264068711929,-0.49,1.4));
#10532=CARTESIAN_POINT('',(4.12047276989058,-0.49,1.51090536506409));
#10533=CARTESIAN_POINT('',(4.12047276989058,-0.49,1.28909463493591));
#10534=CARTESIAN_POINT('',(4.12047276989058,-0.49,1.));
#10535=CARTESIAN_POINT('',(4.07764068711929,-0.49,1.4));
#10536=CARTESIAN_POINT('Origin',(4.24264068711929,-0.49,1.4));
#10537=CARTESIAN_POINT('Origin',(4.24264068711929,-0.49,1.4));
#10538=CARTESIAN_POINT('Origin',(4.24264068711929,-1.,1.4));
#10539=CARTESIAN_POINT('',(4.07764068711929,-0.884745726183518,1.4));
#10540=CARTESIAN_POINT('Ctrl Pts',(4.07764068711929,-0.884745726183518,
1.4));
#10541=CARTESIAN_POINT('Ctrl Pts',(4.07764068711929,-0.884745726183518,
1.42076875940744));
#10542=CARTESIAN_POINT('Ctrl Pts',(4.0818009681117,-0.885552759505265,1.44288889507334));
#10543=CARTESIAN_POINT('Ctrl Pts',(4.0986542169026,-0.888448648150043,1.48352706263377));
#10544=CARTESIAN_POINT('Ctrl Pts',(4.1113446933051,-0.890493604851638,1.50204924397737));
#10545=CARTESIAN_POINT('Ctrl Pts',(4.14059086811116,-0.894317234323941,
1.53129541878344));
#10546=CARTESIAN_POINT('Ctrl Pts',(4.1591132950286,-0.896347088899543,1.54398634598358));
#10547=CARTESIAN_POINT('Ctrl Pts',(4.19975231102587,-0.899208271860583,
1.56083992183864));
#10548=CARTESIAN_POINT('Ctrl Pts',(4.22187274439578,-0.9,1.565));
#10549=CARTESIAN_POINT('Ctrl Pts',(4.26340862984279,-0.9,1.565));
#10550=CARTESIAN_POINT('Ctrl Pts',(4.2855290632127,-0.899208271860583,1.56083992183864));
#10551=CARTESIAN_POINT('Ctrl Pts',(4.32616807920997,-0.896347088899543,
1.54398634598358));
#10552=CARTESIAN_POINT('Ctrl Pts',(4.34469050612741,-0.894317234323941,
1.53129541878344));
#10553=CARTESIAN_POINT('Ctrl Pts',(4.37393668093347,-0.890493604851638,
1.50204924397737));
#10554=CARTESIAN_POINT('Ctrl Pts',(4.38662715733598,-0.888448648150043,
1.48352706263377));
#10555=CARTESIAN_POINT('Ctrl Pts',(4.40348040612687,-0.885552759505265,
1.44288889507334));
#10556=CARTESIAN_POINT('Ctrl Pts',(4.40764068711929,-0.884745726183518,
1.42076875940744));
#10557=CARTESIAN_POINT('Ctrl Pts',(4.40764068711929,-0.884745726183518,
1.37923124059256));
#10558=CARTESIAN_POINT('Ctrl Pts',(4.40348040612687,-0.885552759505265,
1.35711110492666));
#10559=CARTESIAN_POINT('Ctrl Pts',(4.38662715733598,-0.888448648150043,
1.31647293736623));
#10560=CARTESIAN_POINT('Ctrl Pts',(4.37393668093347,-0.890493604851638,
1.29795075602263));
#10561=CARTESIAN_POINT('Ctrl Pts',(4.34469050612741,-0.894317234323941,
1.26870458121656));
#10562=CARTESIAN_POINT('Ctrl Pts',(4.32616807920997,-0.896347088899543,
1.25601365401642));
#10563=CARTESIAN_POINT('Ctrl Pts',(4.2855290632127,-0.899208271860583,1.23916007816136));
#10564=CARTESIAN_POINT('Ctrl Pts',(4.26340862984279,-0.9,1.235));
#10565=CARTESIAN_POINT('Ctrl Pts',(4.22187274439578,-0.9,1.235));
#10566=CARTESIAN_POINT('Ctrl Pts',(4.19975231102587,-0.899208271860583,
1.23916007816136));
#10567=CARTESIAN_POINT('Ctrl Pts',(4.1591132950286,-0.896347088899543,1.25601365401642));
#10568=CARTESIAN_POINT('Ctrl Pts',(4.14059086811116,-0.894317234323941,
1.26870458121656));
#10569=CARTESIAN_POINT('Ctrl Pts',(4.1113446933051,-0.890493604851638,1.29795075602263));
#10570=CARTESIAN_POINT('Ctrl Pts',(4.0986542169026,-0.888448648150043,1.31647293736623));
#10571=CARTESIAN_POINT('Ctrl Pts',(4.0818009681117,-0.885552759505265,1.35711110492666));
#10572=CARTESIAN_POINT('Ctrl Pts',(4.07764068711929,-0.884745726183518,
1.37923124059256));
#10573=CARTESIAN_POINT('Ctrl Pts',(4.07764068711929,-0.884745726183518,
1.4));
#10574=CARTESIAN_POINT('',(4.07764068711929,-1.,1.4));
#10575=CARTESIAN_POINT('',(4.36480860434799,-0.49,1.51090536506409));
#10576=CARTESIAN_POINT('Ctrl Pts',(4.36480860434799,-0.49,1.51090536506409));
#10577=CARTESIAN_POINT('Ctrl Pts',(4.36300960074558,-0.490448531679987,
1.51288705930464));
#10578=CARTESIAN_POINT('Ctrl Pts',(4.36117558368452,-0.490895245371684,
1.51481034122633));
#10579=CARTESIAN_POINT('Ctrl Pts',(4.34475268013864,-0.494795015531646,
1.5312332447722));
#10580=CARTESIAN_POINT('Ctrl Pts',(4.32630040214172,-0.498442514607594,
1.54390845611142));
#10581=CARTESIAN_POINT('Ctrl Pts',(4.28569028316644,-0.50357781976106,1.56079590960766));
#10582=CARTESIAN_POINT('Ctrl Pts',(4.26352078145003,-0.505,1.565));
#10583=CARTESIAN_POINT('Ctrl Pts',(4.22176059278855,-0.505,1.565));
#10584=CARTESIAN_POINT('Ctrl Pts',(4.19959109107213,-0.50357781976106,1.56079590960766));
#10585=CARTESIAN_POINT('Ctrl Pts',(4.15898097209685,-0.498442514607594,
1.54390845611142));
#10586=CARTESIAN_POINT('Ctrl Pts',(4.14052869409993,-0.494795015531646,
1.5312332447722));
#10587=CARTESIAN_POINT('Ctrl Pts',(4.12410579055406,-0.490895245371684,
1.51481034122633));
#10588=CARTESIAN_POINT('Ctrl Pts',(4.12227177349299,-0.490448531679987,
1.51288705930464));
#10589=CARTESIAN_POINT('Ctrl Pts',(4.12047276989058,-0.49,1.51090536506409));
#10590=CARTESIAN_POINT('',(4.36480860434799,-0.49,1.28909463493591));
#10591=CARTESIAN_POINT('Origin',(4.24264068711929,-0.49,1.4));
#10592=CARTESIAN_POINT('Ctrl Pts',(4.12047276989058,-0.49,1.28909463493591));
#10593=CARTESIAN_POINT('Ctrl Pts',(4.12227177349299,-0.490448531679987,
1.28711294069536));
#10594=CARTESIAN_POINT('Ctrl Pts',(4.12410579055406,-0.490895245371684,
1.28518965877367));
#10595=CARTESIAN_POINT('Ctrl Pts',(4.14052869409993,-0.494795015531646,
1.2687667552278));
#10596=CARTESIAN_POINT('Ctrl Pts',(4.15898097209685,-0.498442514607594,
1.25609154388858));
#10597=CARTESIAN_POINT('Ctrl Pts',(4.19959109107213,-0.50357781976106,1.23920409039234));
#10598=CARTESIAN_POINT('Ctrl Pts',(4.22176059278855,-0.505,1.235));
#10599=CARTESIAN_POINT('Ctrl Pts',(4.26352078145003,-0.505,1.235));
#10600=CARTESIAN_POINT('Ctrl Pts',(4.28569028316644,-0.50357781976106,1.23920409039234));
#10601=CARTESIAN_POINT('Ctrl Pts',(4.32630040214172,-0.498442514607594,
1.25609154388858));
#10602=CARTESIAN_POINT('Ctrl Pts',(4.34475268013864,-0.494795015531646,
1.2687667552278));
#10603=CARTESIAN_POINT('Ctrl Pts',(4.36117558368452,-0.490895245371684,
1.28518965877367));
#10604=CARTESIAN_POINT('Ctrl Pts',(4.36300960074558,-0.490448531679987,
1.28711294069536));
#10605=CARTESIAN_POINT('Ctrl Pts',(4.36480860434799,-0.49,1.28909463493591));
#10606=CARTESIAN_POINT('Origin',(4.24264068711929,-0.49,1.4));
#10607=CARTESIAN_POINT('',(4.36480860434799,-0.49,1.));
#10608=CARTESIAN_POINT('Origin',(3.75264069,0.,1.4));
#10609=CARTESIAN_POINT('',(3.75264069,0.122167928782887,1.51090535233657));
#10610=CARTESIAN_POINT('',(3.75264069,0.122167928782887,1.28909464766343));
#10611=CARTESIAN_POINT('',(3.75264069,0.122167928782887,1.));
#10612=CARTESIAN_POINT('Origin',(3.75264069,0.,1.4));
#10613=CARTESIAN_POINT('Origin',(3.24264069,0.,1.4));
#10614=CARTESIAN_POINT('',(3.35789496093577,0.165,1.4));
#10615=CARTESIAN_POINT('',(3.34264068711929,-2.02066721859313E-17,1.565));
#10616=CARTESIAN_POINT('Ctrl Pts',(3.35789496093577,0.165,1.4));
#10617=CARTESIAN_POINT('Ctrl Pts',(3.35789496093577,0.165,1.42076875940744));
#10618=CARTESIAN_POINT('Ctrl Pts',(3.35708792761402,0.160839719007584,1.44288889507334));
#10619=CARTESIAN_POINT('Ctrl Pts',(3.35419203896924,0.143986470216691,1.48352706263377));
#10620=CARTESIAN_POINT('Ctrl Pts',(3.35214708226765,0.131295993814186,1.50204924397737));
#10621=CARTESIAN_POINT('Ctrl Pts',(3.34832345279534,0.102049819008125,1.53129541878344));
#10622=CARTESIAN_POINT('Ctrl Pts',(3.34629359821974,0.0835273920906824,
1.54398634598358));
#10623=CARTESIAN_POINT('Ctrl Pts',(3.3434324152587,0.0428883760934127,1.56083992183864));
#10624=CARTESIAN_POINT('Ctrl Pts',(3.34264068711929,0.0207679427235068,
1.565));
#10625=CARTESIAN_POINT('Ctrl Pts',(3.34264068711929,2.77555756156289E-17,
1.565));
#10626=CARTESIAN_POINT('',(3.34264068711929,-7.59257876733526E-17,1.235));
#10627=CARTESIAN_POINT('Ctrl Pts',(3.34264068711929,-4.16333634234434E-17,
1.235));
#10628=CARTESIAN_POINT('Ctrl Pts',(3.34264068711929,0.0207679427235068,
1.235));
#10629=CARTESIAN_POINT('Ctrl Pts',(3.3434324152587,0.0428883760934127,1.23916007816136));
#10630=CARTESIAN_POINT('Ctrl Pts',(3.34629359821974,0.0835273920906823,
1.25601365401642));
#10631=CARTESIAN_POINT('Ctrl Pts',(3.34832345279534,0.102049819008125,1.26870458121656));
#10632=CARTESIAN_POINT('Ctrl Pts',(3.35214708226765,0.131295993814186,1.29795075602263));
#10633=CARTESIAN_POINT('Ctrl Pts',(3.35419203896924,0.143986470216691,1.31647293736623));
#10634=CARTESIAN_POINT('Ctrl Pts',(3.35708792761402,0.160839719007584,1.35711110492666));
#10635=CARTESIAN_POINT('Ctrl Pts',(3.35789496093577,0.165,1.37923124059256));
#10636=CARTESIAN_POINT('Ctrl Pts',(3.35789496093577,0.165,1.4));
#10637=CARTESIAN_POINT('Ctrl Pts',(3.34264068711929,2.77555756156289E-17,
1.565));
#10638=CARTESIAN_POINT('Ctrl Pts',(3.34264068711929,-0.0207679427235068,
1.565));
#10639=CARTESIAN_POINT('Ctrl Pts',(3.3434324152587,-0.0428883760934127,
1.56083992183864));
#10640=CARTESIAN_POINT('Ctrl Pts',(3.34629359821974,-0.0835273920906823,
1.54398634598358));
#10641=CARTESIAN_POINT('Ctrl Pts',(3.34832345279534,-0.102049819008125,
1.53129541878344));
#10642=CARTESIAN_POINT('Ctrl Pts',(3.35214708226765,-0.131295993814186,
1.50204924397737));
#10643=CARTESIAN_POINT('Ctrl Pts',(3.35419203896924,-0.143986470216691,
1.48352706263377));
#10644=CARTESIAN_POINT('Ctrl Pts',(3.35708792761402,-0.160839719007584,
1.44288889507334));
#10645=CARTESIAN_POINT('Ctrl Pts',(3.35789496093577,-0.165,1.42076875940744));
#10646=CARTESIAN_POINT('Ctrl Pts',(3.35789496093577,-0.165,1.37923124059256));
#10647=CARTESIAN_POINT('Ctrl Pts',(3.35708792761402,-0.160839719007584,
1.35711110492666));
#10648=CARTESIAN_POINT('Ctrl Pts',(3.35419203896924,-0.143986470216691,
1.31647293736623));
#10649=CARTESIAN_POINT('Ctrl Pts',(3.35214708226765,-0.131295993814186,
1.29795075602263));
#10650=CARTESIAN_POINT('Ctrl Pts',(3.34832345279534,-0.102049819008125,
1.26870458121656));
#10651=CARTESIAN_POINT('Ctrl Pts',(3.34629359821974,-0.0835273920906824,
1.25601365401642));
#10652=CARTESIAN_POINT('Ctrl Pts',(3.3434324152587,-0.0428883760934128,
1.23916007816136));
#10653=CARTESIAN_POINT('Ctrl Pts',(3.34264068711929,-0.0207679427235068,
1.235));
#10654=CARTESIAN_POINT('Ctrl Pts',(3.34264068711929,-4.16333634234434E-17,
1.235));
#10655=CARTESIAN_POINT('',(3.73764068711929,-1.70422299968729E-17,1.565));
#10656=CARTESIAN_POINT('',(3.24264069,-2.02066721859313E-17,1.565));
#10657=CARTESIAN_POINT('',(3.75264069,-0.122167928782887,1.51090535233657));
#10658=CARTESIAN_POINT('Ctrl Pts',(3.75264069,-0.122167928782887,1.51090535233657));
#10659=CARTESIAN_POINT('Ctrl Pts',(3.75219215735201,-0.120368921478644,
1.51288705106972));
#10660=CARTESIAN_POINT('Ctrl Pts',(3.75174544269427,-0.118534900551874,
1.51481033723969));
#10661=CARTESIAN_POINT('Ctrl Pts',(3.74784567158764,-0.102111993019358,
1.5312332447722));
#10662=CARTESIAN_POINT('Ctrl Pts',(3.74419817251169,-0.0836597150224319,
1.54390845611142));
#10663=CARTESIAN_POINT('Ctrl Pts',(3.73906286735823,-0.0430495960471595,
1.56079590960766));
#10664=CARTESIAN_POINT('Ctrl Pts',(3.73764068711929,-0.020880094330741,
1.565));
#10665=CARTESIAN_POINT('Ctrl Pts',(3.73764068711929,-2.08166817117217E-17,
1.565));
#10666=CARTESIAN_POINT('',(3.75264069,-0.122167928782887,1.28909464766343));
#10667=CARTESIAN_POINT('Origin',(3.75264069,0.,1.4));
#10668=CARTESIAN_POINT('',(3.73764068711929,-3.09223316784707E-17,1.235));
#10669=CARTESIAN_POINT('Ctrl Pts',(3.73764068711929,-1.38777878078145E-17,
1.235));
#10670=CARTESIAN_POINT('Ctrl Pts',(3.73764068711929,-0.020880094330741,
1.235));
#10671=CARTESIAN_POINT('Ctrl Pts',(3.73906286735823,-0.0430495960471595,
1.23920409039234));
#10672=CARTESIAN_POINT('Ctrl Pts',(3.74419817251169,-0.0836597150224319,
1.25609154388858));
#10673=CARTESIAN_POINT('Ctrl Pts',(3.74784567158764,-0.102111993019358,
1.2687667552278));
#10674=CARTESIAN_POINT('Ctrl Pts',(3.75174544269427,-0.118534900551874,
1.28518966276031));
#10675=CARTESIAN_POINT('Ctrl Pts',(3.75219215735201,-0.120368921478644,
1.28711294893028));
#10676=CARTESIAN_POINT('Ctrl Pts',(3.75264069,-0.122167928782887,1.28909464766343));
#10677=CARTESIAN_POINT('Ctrl Pts',(3.75264069,0.122167928782887,1.28909464766343));
#10678=CARTESIAN_POINT('Ctrl Pts',(3.75219215735201,0.120368921478644,1.28711294893028));
#10679=CARTESIAN_POINT('Ctrl Pts',(3.75174544269427,0.118534900551874,1.28518966276031));
#10680=CARTESIAN_POINT('Ctrl Pts',(3.74784567158764,0.102111993019358,1.2687667552278));
#10681=CARTESIAN_POINT('Ctrl Pts',(3.74419817251169,0.0836597150224319,
1.25609154388858));
#10682=CARTESIAN_POINT('Ctrl Pts',(3.73906286735823,0.0430495960471595,
1.23920409039234));
#10683=CARTESIAN_POINT('Ctrl Pts',(3.73764068711929,0.020880094330741,1.235));
#10684=CARTESIAN_POINT('Ctrl Pts',(3.73764068711929,0.,1.235));
#10685=CARTESIAN_POINT('Ctrl Pts',(3.73764068711929,-6.93889390390723E-18,
1.565));
#10686=CARTESIAN_POINT('Ctrl Pts',(3.73764068711929,0.020880094330741,1.565));
#10687=CARTESIAN_POINT('Ctrl Pts',(3.73906286735823,0.0430495960471595,
1.56079590960766));
#10688=CARTESIAN_POINT('Ctrl Pts',(3.74419817251169,0.0836597150224318,
1.54390845611142));
#10689=CARTESIAN_POINT('Ctrl Pts',(3.74784567158764,0.102111993019358,1.5312332447722));
#10690=CARTESIAN_POINT('Ctrl Pts',(3.75174544269427,0.118534900551874,1.51481033723969));
#10691=CARTESIAN_POINT('Ctrl Pts',(3.75219215735201,0.120368921478644,1.51288705106972));
#10692=CARTESIAN_POINT('Ctrl Pts',(3.75264069,0.122167928782887,1.51090535233657));
#10693=CARTESIAN_POINT('Origin',(3.75264069,0.,1.4));
#10694=CARTESIAN_POINT('',(3.75264069,-0.122167928782887,1.));
#10695=CARTESIAN_POINT('Origin',(4.24264068711929,0.,1.));
#10696=CARTESIAN_POINT('',(3.73764068711929,-6.18446633569413E-17,1.8));
#10697=CARTESIAN_POINT('Origin',(4.24264068711929,0.,1.8));
#10698=CARTESIAN_POINT('',(3.73764068711929,-6.18446633569413E-17,1.));
#10699=CARTESIAN_POINT('',(3.73764068711929,-6.18446633569413E-17,1.));
#10700=CARTESIAN_POINT('',(3.73764068711929,-6.18446633569413E-17,1.));
#10701=CARTESIAN_POINT('Origin',(4.24264068711929,0.,1.));
#10702=CARTESIAN_POINT('Origin',(4.24264068711929,0.,1.));
#10703=CARTESIAN_POINT('',(3.34264068711929,-1.10218211923262E-16,1.8));
#10704=CARTESIAN_POINT('Origin',(4.24264068711929,0.,1.8));
#10705=CARTESIAN_POINT('',(3.34264068711929,-1.10218211923262E-16,1.));
#10706=CARTESIAN_POINT('',(3.34264068711929,-1.10218211923262E-16,1.));
#10707=CARTESIAN_POINT('',(3.34264068711929,-1.10218211923262E-16,1.));
#10708=CARTESIAN_POINT('Origin',(4.24264068711929,0.,1.));
#10709=CARTESIAN_POINT('Origin',(4.24264068711929,0.,1.8));
#10710=CARTESIAN_POINT('Origin',(4.24264068711929,0.,1.));
#10711=CARTESIAN_POINT('',(0.,0.,0.));
#10712=CARTESIAN_POINT('Origin',(0.,-0.4,0.));
#10713=CARTESIAN_POINT('',(-0.1954,-0.4,2.39295984553393E-17));
#10714=CARTESIAN_POINT('Origin',(0.,-0.4,0.));
#10715=CARTESIAN_POINT('Origin',(0.0577350269189626,0.,-0.1));
#10716=CARTESIAN_POINT('',(0.0577350269189626,0.,-0.1));
#10717=CARTESIAN_POINT('',(0.115470053837925,0.,0.));
#10718=CARTESIAN_POINT('',(0.0934187836487032,0.,-0.0381939203391614));
#10719=CARTESIAN_POINT('',(0.0577350269189626,-0.2,-0.1));
#10720=CARTESIAN_POINT('',(0.0577350269189626,0.,-0.1));
#10721=CARTESIAN_POINT('',(0.115470053837925,-0.2,0.));
#10722=CARTESIAN_POINT('',(0.115470053837925,-0.2,0.));
#10723=CARTESIAN_POINT('',(0.115470053837925,0.,0.));
#10724=CARTESIAN_POINT('Origin',(-0.0577350269189626,0.,-0.1));
#10725=CARTESIAN_POINT('',(-0.0577350269189626,0.,-0.1));
#10726=CARTESIAN_POINT('',(0.0561324865405187,0.,-0.1));
#10727=CARTESIAN_POINT('',(-0.0577350269189626,-0.2,-0.1));
#10728=CARTESIAN_POINT('',(-0.0577350269189626,0.,-0.1));
#10729=CARTESIAN_POINT('',(0.0577350269189626,-0.2,-0.1));
#10730=CARTESIAN_POINT('Origin',(-0.115470053837925,0.,-1.38777878078145E-17));
#10731=CARTESIAN_POINT('',(-0.115470053837925,0.,-1.41410031829988E-17));
#10732=CARTESIAN_POINT('',(-0.0797862971081845,0.,-0.0618060796608387));
#10733=CARTESIAN_POINT('',(-0.115470053837925,-0.2,-1.38777878078145E-17));
#10734=CARTESIAN_POINT('',(-0.115470053837925,0.,-1.41410031829988E-17));
#10735=CARTESIAN_POINT('',(-0.0577350269189626,-0.2,-0.1));
#10736=CARTESIAN_POINT('Origin',(-0.0577350269189626,0.,0.1));
#10737=CARTESIAN_POINT('',(-0.0577350269189626,0.,0.1));
#10738=CARTESIAN_POINT('',(-0.0509187836487033,0.,0.111806079660839));
#10739=CARTESIAN_POINT('',(-0.0577350269189626,-0.2,0.1));
#10740=CARTESIAN_POINT('',(-0.0577350269189626,0.,0.1));
#10741=CARTESIAN_POINT('',(-0.115470053837925,-0.2,-1.41410031829988E-17));
#10742=CARTESIAN_POINT('Origin',(0.0577350269189626,0.,0.1));
#10743=CARTESIAN_POINT('',(0.0577350269189626,0.,0.1));
#10744=CARTESIAN_POINT('',(0.113867513459481,0.,0.1));
#10745=CARTESIAN_POINT('',(0.0577350269189626,-0.2,0.1));
#10746=CARTESIAN_POINT('',(0.0577350269189626,0.,0.1));
#10747=CARTESIAN_POINT('',(-0.0577350269189626,-0.2,0.1));
#10748=CARTESIAN_POINT('Origin',(0.115470053837925,0.,0.));
#10749=CARTESIAN_POINT('',(0.122286297108185,0.,-0.0118060796608386));
#10750=CARTESIAN_POINT('',(0.0577350269189626,-0.2,0.1));
#10751=CARTESIAN_POINT('Origin',(0.,-0.2,0.));
#10752=CARTESIAN_POINT('Origin',(0.17,0.,0.));
#10753=CARTESIAN_POINT('',(-0.17,-8.67361737988404E-18,-2.0818995585505E-17));
#10754=CARTESIAN_POINT('Origin',(0.,0.,0.));
#10755=CARTESIAN_POINT('Origin',(0.,-0.015,0.));
#10756=CARTESIAN_POINT('',(-0.1954,-0.0254,-2.39295984553393E-17));
#10757=CARTESIAN_POINT('Origin',(0.,-0.0254,0.));
#10758=CARTESIAN_POINT('',(-0.185,-0.015,-2.2655965784226E-17));
#10759=CARTESIAN_POINT('Origin',(0.,-0.2775,0.));
#10760=CARTESIAN_POINT('',(-0.1954,-0.2775,-2.39295984553393E-17));
#10761=CARTESIAN_POINT('',(0.,0.,0.));
#10762=CARTESIAN_POINT('',(0.,0.,0.));
#10763=CARTESIAN_POINT('',(0.,0.,0.));
#10764=CARTESIAN_POINT('',(0.,0.,0.));
#10765=CARTESIAN_POINT('',(0.,0.,0.));
#10766=CARTESIAN_POINT('',(0.,0.,0.));
#10767=CARTESIAN_POINT('',(0.,0.,0.));
#10768=CARTESIAN_POINT('',(0.,0.,0.));
#10769=CARTESIAN_POINT('',(0.,-0.9,1.4));
#10770=CARTESIAN_POINT('',(0.,0.,7.));
#10771=CARTESIAN_POINT('',(0.,0.,0.));
#10772=CARTESIAN_POINT('',(0.,0.,0.));
#10773=CARTESIAN_POINT('',(0.,0.,0.));
#10774=CARTESIAN_POINT('',(4.24264068711929,-0.9,1.4));
#10775=CARTESIAN_POINT('',(0.,0.,0.));
#10776=CARTESIAN_POINT('',(0.,0.,0.));
#10777=CARTESIAN_POINT('',(0.0070716531291544,-0.244857016039734,0.));
#10778=UNCERTAINTY_MEASURE_WITH_UNIT(LENGTH_MEASURE(0.001),#10838,
'DISTANCE_ACCURACY_VALUE',
'Maximum model space distance between geometric entities at asserted c
onnectivities');
#10779=UNCERTAINTY_MEASURE_WITH_UNIT(LENGTH_MEASURE(0.001),#10838,
'DISTANCE_ACCURACY_VALUE',
'Maximum model space distance between geometric entities at asserted c
onnectivities');
#10780=UNCERTAINTY_MEASURE_WITH_UNIT(LENGTH_MEASURE(0.001),#10838,
'DISTANCE_ACCURACY_VALUE',
'Maximum model space distance between geometric entities at asserted c
onnectivities');
#10781=UNCERTAINTY_MEASURE_WITH_UNIT(LENGTH_MEASURE(0.001),#10838,
'DISTANCE_ACCURACY_VALUE',
'Maximum model space distance between geometric entities at asserted c
onnectivities');
#10782=UNCERTAINTY_MEASURE_WITH_UNIT(LENGTH_MEASURE(0.001),#10838,
'DISTANCE_ACCURACY_VALUE',
'Maximum model space distance between geometric entities at asserted c
onnectivities');
#10783=UNCERTAINTY_MEASURE_WITH_UNIT(LENGTH_MEASURE(0.001),#10838,
'DISTANCE_ACCURACY_VALUE',
'Maximum model space distance between geometric entities at asserted c
onnectivities');
#10784=UNCERTAINTY_MEASURE_WITH_UNIT(LENGTH_MEASURE(0.001),#10838,
'DISTANCE_ACCURACY_VALUE',
'Maximum model space distance between geometric entities at asserted c
onnectivities');
#10785=UNCERTAINTY_MEASURE_WITH_UNIT(LENGTH_MEASURE(0.001),#10838,
'DISTANCE_ACCURACY_VALUE',
'Maximum model space distance between geometric entities at asserted c
onnectivities');
#10786=UNCERTAINTY_MEASURE_WITH_UNIT(LENGTH_MEASURE(0.001),#10838,
'DISTANCE_ACCURACY_VALUE',
'Maximum model space distance between geometric entities at asserted c
onnectivities');
#10787=UNCERTAINTY_MEASURE_WITH_UNIT(LENGTH_MEASURE(0.001),#10838,
'DISTANCE_ACCURACY_VALUE',
'Maximum model space distance between geometric entities at asserted c
onnectivities');
#10788=UNCERTAINTY_MEASURE_WITH_UNIT(LENGTH_MEASURE(0.001),#10838,
'DISTANCE_ACCURACY_VALUE',
'Maximum model space distance between geometric entities at asserted c
onnectivities');
#10789=UNCERTAINTY_MEASURE_WITH_UNIT(LENGTH_MEASURE(0.001),#10838,
'DISTANCE_ACCURACY_VALUE',
'Maximum model space distance between geometric entities at asserted c
onnectivities');
#10790=UNCERTAINTY_MEASURE_WITH_UNIT(LENGTH_MEASURE(0.001),#10838,
'DISTANCE_ACCURACY_VALUE',
'Maximum model space distance between geometric entities at asserted c
onnectivities');
#10791=UNCERTAINTY_MEASURE_WITH_UNIT(LENGTH_MEASURE(0.001),#10838,
'DISTANCE_ACCURACY_VALUE',
'Maximum model space distance between geometric entities at asserted c
onnectivities');
#10792=UNCERTAINTY_MEASURE_WITH_UNIT(LENGTH_MEASURE(0.001),#10838,
'DISTANCE_ACCURACY_VALUE',
'Maximum model space distance between geometric entities at asserted c
onnectivities');
#10793=UNCERTAINTY_MEASURE_WITH_UNIT(LENGTH_MEASURE(0.001),#10838,
'DISTANCE_ACCURACY_VALUE',
'Maximum model space distance between geometric entities at asserted c
onnectivities');
#10794=UNCERTAINTY_MEASURE_WITH_UNIT(LENGTH_MEASURE(0.001),#10838,
'DISTANCE_ACCURACY_VALUE',
'Maximum model space distance between geometric entities at asserted c
onnectivities');
#10795=UNCERTAINTY_MEASURE_WITH_UNIT(LENGTH_MEASURE(0.001),#10838,
'DISTANCE_ACCURACY_VALUE',
'Maximum model space distance between geometric entities at asserted c
onnectivities');
#10796=UNCERTAINTY_MEASURE_WITH_UNIT(LENGTH_MEASURE(0.001),#10838,
'DISTANCE_ACCURACY_VALUE',
'Maximum model space distance between geometric entities at asserted c
onnectivities');
#10797=UNCERTAINTY_MEASURE_WITH_UNIT(LENGTH_MEASURE(0.001),#10838,
'DISTANCE_ACCURACY_VALUE',
'Maximum model space distance between geometric entities at asserted c
onnectivities');
#10798=UNCERTAINTY_MEASURE_WITH_UNIT(LENGTH_MEASURE(0.001),#10838,
'DISTANCE_ACCURACY_VALUE',
'Maximum model space distance between geometric entities at asserted c
onnectivities');
#10799=UNCERTAINTY_MEASURE_WITH_UNIT(LENGTH_MEASURE(0.001),#10838,
'DISTANCE_ACCURACY_VALUE',
'Maximum model space distance between geometric entities at asserted c
onnectivities');
#10800=UNCERTAINTY_MEASURE_WITH_UNIT(LENGTH_MEASURE(0.001),#10838,
'DISTANCE_ACCURACY_VALUE',
'Maximum model space distance between geometric entities at asserted c
onnectivities');
#10801=UNCERTAINTY_MEASURE_WITH_UNIT(LENGTH_MEASURE(0.001),#10838,
'DISTANCE_ACCURACY_VALUE',
'Maximum model space distance between geometric entities at asserted c
onnectivities');
#10802=UNCERTAINTY_MEASURE_WITH_UNIT(LENGTH_MEASURE(0.001),#10838,
'DISTANCE_ACCURACY_VALUE',
'Maximum model space distance between geometric entities at asserted c
onnectivities');
#10803=UNCERTAINTY_MEASURE_WITH_UNIT(LENGTH_MEASURE(0.001),#10838,
'DISTANCE_ACCURACY_VALUE',
'Maximum model space distance between geometric entities at asserted c
onnectivities');
#10804=UNCERTAINTY_MEASURE_WITH_UNIT(LENGTH_MEASURE(0.001),#10838,
'DISTANCE_ACCURACY_VALUE',
'Maximum model space distance between geometric entities at asserted c
onnectivities');
#10805=UNCERTAINTY_MEASURE_WITH_UNIT(LENGTH_MEASURE(0.001),#10838,
'DISTANCE_ACCURACY_VALUE',
'Maximum model space distance between geometric entities at asserted c
onnectivities');
#10806=UNCERTAINTY_MEASURE_WITH_UNIT(LENGTH_MEASURE(0.001),#10838,
'DISTANCE_ACCURACY_VALUE',
'Maximum model space distance between geometric entities at asserted c
onnectivities');
#10807=UNCERTAINTY_MEASURE_WITH_UNIT(LENGTH_MEASURE(0.001),#10838,
'DISTANCE_ACCURACY_VALUE',
'Maximum model space distance between geometric entities at asserted c
onnectivities');
#10808=(
GEOMETRIC_REPRESENTATION_CONTEXT(3)
GLOBAL_UNCERTAINTY_ASSIGNED_CONTEXT((#10778))
GLOBAL_UNIT_ASSIGNED_CONTEXT((#10838,#10840,#10841))
REPRESENTATION_CONTEXT('','3D')
);
#10809=(
GEOMETRIC_REPRESENTATION_CONTEXT(3)
GLOBAL_UNCERTAINTY_ASSIGNED_CONTEXT((#10779))
GLOBAL_UNIT_ASSIGNED_CONTEXT((#10838,#10840,#10841))
REPRESENTATION_CONTEXT('','3D')
);
#10810=(
GEOMETRIC_REPRESENTATION_CONTEXT(3)
GLOBAL_UNCERTAINTY_ASSIGNED_CONTEXT((#10780))
GLOBAL_UNIT_ASSIGNED_CONTEXT((#10838,#10840,#10841))
REPRESENTATION_CONTEXT('','3D')
);
#10811=(
GEOMETRIC_REPRESENTATION_CONTEXT(3)
GLOBAL_UNCERTAINTY_ASSIGNED_CONTEXT((#10781))
GLOBAL_UNIT_ASSIGNED_CONTEXT((#10838,#10840,#10841))
REPRESENTATION_CONTEXT('','3D')
);
#10812=(
GEOMETRIC_REPRESENTATION_CONTEXT(3)
GLOBAL_UNCERTAINTY_ASSIGNED_CONTEXT((#10782))
GLOBAL_UNIT_ASSIGNED_CONTEXT((#10838,#10840,#10841))
REPRESENTATION_CONTEXT('','3D')
);
#10813=(
GEOMETRIC_REPRESENTATION_CONTEXT(3)
GLOBAL_UNCERTAINTY_ASSIGNED_CONTEXT((#10783))
GLOBAL_UNIT_ASSIGNED_CONTEXT((#10838,#10840,#10841))
REPRESENTATION_CONTEXT('','3D')
);
#10814=(
GEOMETRIC_REPRESENTATION_CONTEXT(3)
GLOBAL_UNCERTAINTY_ASSIGNED_CONTEXT((#10784))
GLOBAL_UNIT_ASSIGNED_CONTEXT((#10838,#10840,#10841))
REPRESENTATION_CONTEXT('','3D')
);
#10815=(
GEOMETRIC_REPRESENTATION_CONTEXT(3)
GLOBAL_UNCERTAINTY_ASSIGNED_CONTEXT((#10785))
GLOBAL_UNIT_ASSIGNED_CONTEXT((#10838,#10840,#10841))
REPRESENTATION_CONTEXT('','3D')
);
#10816=(
GEOMETRIC_REPRESENTATION_CONTEXT(3)
GLOBAL_UNCERTAINTY_ASSIGNED_CONTEXT((#10786))
GLOBAL_UNIT_ASSIGNED_CONTEXT((#10838,#10840,#10841))
REPRESENTATION_CONTEXT('','3D')
);
#10817=(
GEOMETRIC_REPRESENTATION_CONTEXT(3)
GLOBAL_UNCERTAINTY_ASSIGNED_CONTEXT((#10787))
GLOBAL_UNIT_ASSIGNED_CONTEXT((#10838,#10840,#10841))
REPRESENTATION_CONTEXT('','3D')
);
#10818=(
GEOMETRIC_REPRESENTATION_CONTEXT(3)
GLOBAL_UNCERTAINTY_ASSIGNED_CONTEXT((#10788))
GLOBAL_UNIT_ASSIGNED_CONTEXT((#10838,#10840,#10841))
REPRESENTATION_CONTEXT('','3D')
);
#10819=(
GEOMETRIC_REPRESENTATION_CONTEXT(3)
GLOBAL_UNCERTAINTY_ASSIGNED_CONTEXT((#10789))
GLOBAL_UNIT_ASSIGNED_CONTEXT((#10838,#10840,#10841))
REPRESENTATION_CONTEXT('','3D')
);
#10820=(
GEOMETRIC_REPRESENTATION_CONTEXT(3)
GLOBAL_UNCERTAINTY_ASSIGNED_CONTEXT((#10790))
GLOBAL_UNIT_ASSIGNED_CONTEXT((#10838,#10840,#10841))
REPRESENTATION_CONTEXT('','3D')
);
#10821=(
GEOMETRIC_REPRESENTATION_CONTEXT(3)
GLOBAL_UNCERTAINTY_ASSIGNED_CONTEXT((#10791))
GLOBAL_UNIT_ASSIGNED_CONTEXT((#10838,#10840,#10841))
REPRESENTATION_CONTEXT('','3D')
);
#10822=(
GEOMETRIC_REPRESENTATION_CONTEXT(3)
GLOBAL_UNCERTAINTY_ASSIGNED_CONTEXT((#10792))
GLOBAL_UNIT_ASSIGNED_CONTEXT((#10838,#10840,#10841))
REPRESENTATION_CONTEXT('','3D')
);
#10823=(
GEOMETRIC_REPRESENTATION_CONTEXT(3)
GLOBAL_UNCERTAINTY_ASSIGNED_CONTEXT((#10793))
GLOBAL_UNIT_ASSIGNED_CONTEXT((#10838,#10840,#10841))
REPRESENTATION_CONTEXT('','3D')
);
#10824=(
GEOMETRIC_REPRESENTATION_CONTEXT(3)
GLOBAL_UNCERTAINTY_ASSIGNED_CONTEXT((#10794))
GLOBAL_UNIT_ASSIGNED_CONTEXT((#10838,#10840,#10841))
REPRESENTATION_CONTEXT('','3D')
);
#10825=(
GEOMETRIC_REPRESENTATION_CONTEXT(3)
GLOBAL_UNCERTAINTY_ASSIGNED_CONTEXT((#10795))
GLOBAL_UNIT_ASSIGNED_CONTEXT((#10838,#10840,#10841))
REPRESENTATION_CONTEXT('','3D')
);
#10826=(
GEOMETRIC_REPRESENTATION_CONTEXT(3)
GLOBAL_UNCERTAINTY_ASSIGNED_CONTEXT((#10796))
GLOBAL_UNIT_ASSIGNED_CONTEXT((#10838,#10840,#10841))
REPRESENTATION_CONTEXT('','3D')
);
#10827=(
GEOMETRIC_REPRESENTATION_CONTEXT(3)
GLOBAL_UNCERTAINTY_ASSIGNED_CONTEXT((#10797))
GLOBAL_UNIT_ASSIGNED_CONTEXT((#10838,#10840,#10841))
REPRESENTATION_CONTEXT('','3D')
);
#10828=(
GEOMETRIC_REPRESENTATION_CONTEXT(3)
GLOBAL_UNCERTAINTY_ASSIGNED_CONTEXT((#10798))
GLOBAL_UNIT_ASSIGNED_CONTEXT((#10838,#10840,#10841))
REPRESENTATION_CONTEXT('','3D')
);
#10829=(
GEOMETRIC_REPRESENTATION_CONTEXT(3)
GLOBAL_UNCERTAINTY_ASSIGNED_CONTEXT((#10799))
GLOBAL_UNIT_ASSIGNED_CONTEXT((#10838,#10840,#10841))
REPRESENTATION_CONTEXT('','3D')
);
#10830=(
GEOMETRIC_REPRESENTATION_CONTEXT(3)
GLOBAL_UNCERTAINTY_ASSIGNED_CONTEXT((#10800))
GLOBAL_UNIT_ASSIGNED_CONTEXT((#10838,#10840,#10841))
REPRESENTATION_CONTEXT('','3D')
);
#10831=(
GEOMETRIC_REPRESENTATION_CONTEXT(3)
GLOBAL_UNCERTAINTY_ASSIGNED_CONTEXT((#10801))
GLOBAL_UNIT_ASSIGNED_CONTEXT((#10838,#10840,#10841))
REPRESENTATION_CONTEXT('','3D')
);
#10832=(
GEOMETRIC_REPRESENTATION_CONTEXT(3)
GLOBAL_UNCERTAINTY_ASSIGNED_CONTEXT((#10802))
GLOBAL_UNIT_ASSIGNED_CONTEXT((#10838,#10840,#10841))
REPRESENTATION_CONTEXT('','3D')
);
#10833=(
GEOMETRIC_REPRESENTATION_CONTEXT(3)
GLOBAL_UNCERTAINTY_ASSIGNED_CONTEXT((#10803))
GLOBAL_UNIT_ASSIGNED_CONTEXT((#10838,#10840,#10841))
REPRESENTATION_CONTEXT('','3D')
);
#10834=(
GEOMETRIC_REPRESENTATION_CONTEXT(3)
GLOBAL_UNCERTAINTY_ASSIGNED_CONTEXT((#10804))
GLOBAL_UNIT_ASSIGNED_CONTEXT((#10838,#10840,#10841))
REPRESENTATION_CONTEXT('','3D')
);
#10835=(
GEOMETRIC_REPRESENTATION_CONTEXT(3)
GLOBAL_UNCERTAINTY_ASSIGNED_CONTEXT((#10805))
GLOBAL_UNIT_ASSIGNED_CONTEXT((#10838,#10840,#10841))
REPRESENTATION_CONTEXT('','3D')
);
#10836=(
GEOMETRIC_REPRESENTATION_CONTEXT(3)
GLOBAL_UNCERTAINTY_ASSIGNED_CONTEXT((#10806))
GLOBAL_UNIT_ASSIGNED_CONTEXT((#10838,#10840,#10841))
REPRESENTATION_CONTEXT('','3D')
);
#10837=(
GEOMETRIC_REPRESENTATION_CONTEXT(3)
GLOBAL_UNCERTAINTY_ASSIGNED_CONTEXT((#10807))
GLOBAL_UNIT_ASSIGNED_CONTEXT((#10838,#10840,#10841))
REPRESENTATION_CONTEXT('','3D')
);
#10838=(
LENGTH_UNIT()
NAMED_UNIT(*)
SI_UNIT(.CENTI.,.METRE.)
);
#10839=(
LENGTH_UNIT()
NAMED_UNIT(*)
SI_UNIT($,.METRE.)
);
#10840=(
NAMED_UNIT(*)
PLANE_ANGLE_UNIT()
SI_UNIT($,.RADIAN.)
);
#10841=(
NAMED_UNIT(*)
SI_UNIT($,.STERADIAN.)
SOLID_ANGLE_UNIT()
);
#10842=SHAPE_DEFINITION_REPRESENTATION(#10871,#10941);
#10843=SHAPE_DEFINITION_REPRESENTATION(#10872,#10942);
#10844=SHAPE_DEFINITION_REPRESENTATION(#10873,#10943);
#10845=SHAPE_DEFINITION_REPRESENTATION(#10874,#10944);
#10846=SHAPE_DEFINITION_REPRESENTATION(#10875,#10945);
#10847=SHAPE_DEFINITION_REPRESENTATION(#10876,#10946);
#10848=SHAPE_DEFINITION_REPRESENTATION(#10877,#10947);
#10849=SHAPE_DEFINITION_REPRESENTATION(#10878,#10948);
#10850=SHAPE_DEFINITION_REPRESENTATION(#10879,#10949);
#10851=SHAPE_DEFINITION_REPRESENTATION(#10880,#10950);
#10852=SHAPE_DEFINITION_REPRESENTATION(#10881,#10951);
#10853=SHAPE_DEFINITION_REPRESENTATION(#10882,#10952);
#10854=SHAPE_DEFINITION_REPRESENTATION(#10883,#10953);
#10855=SHAPE_DEFINITION_REPRESENTATION(#10884,#10954);
#10856=SHAPE_DEFINITION_REPRESENTATION(#10890,#10955);
#10857=SHAPE_DEFINITION_REPRESENTATION(#10891,#10956);
#10858=SHAPE_DEFINITION_REPRESENTATION(#10892,#10957);
#10859=SHAPE_DEFINITION_REPRESENTATION(#10893,#10958);
#10860=SHAPE_DEFINITION_REPRESENTATION(#10894,#10959);
#10861=SHAPE_DEFINITION_REPRESENTATION(#10895,#10960);
#10862=SHAPE_DEFINITION_REPRESENTATION(#10896,#10961);
#10863=SHAPE_DEFINITION_REPRESENTATION(#10897,#10962);
#10864=SHAPE_DEFINITION_REPRESENTATION(#10898,#10963);
#10865=SHAPE_DEFINITION_REPRESENTATION(#10899,#10964);
#10866=SHAPE_DEFINITION_REPRESENTATION(#10919,#10965);
#10867=SHAPE_DEFINITION_REPRESENTATION(#10920,#10966);
#10868=SHAPE_DEFINITION_REPRESENTATION(#10921,#10967);
#10869=SHAPE_DEFINITION_REPRESENTATION(#10922,#10968);
#10870=SHAPE_DEFINITION_REPRESENTATION(#10923,#10969);
#10871=PRODUCT_DEFINITION_SHAPE('',$,#10971);
#10872=PRODUCT_DEFINITION_SHAPE('',$,#10972);
#10873=PRODUCT_DEFINITION_SHAPE('',$,#10973);
#10874=PRODUCT_DEFINITION_SHAPE('',$,#10974);
#10875=PRODUCT_DEFINITION_SHAPE('',$,#10975);
#10876=PRODUCT_DEFINITION_SHAPE('',$,#10976);
#10877=PRODUCT_DEFINITION_SHAPE('',$,#10977);
#10878=PRODUCT_DEFINITION_SHAPE('',$,#10978);
#10879=PRODUCT_DEFINITION_SHAPE('',$,#10979);
#10880=PRODUCT_DEFINITION_SHAPE('',$,#10980);
#10881=PRODUCT_DEFINITION_SHAPE('',$,#10981);
#10882=PRODUCT_DEFINITION_SHAPE('',$,#10982);
#10883=PRODUCT_DEFINITION_SHAPE('',$,#10983);
#10884=PRODUCT_DEFINITION_SHAPE('',$,#10984);
#10885=PRODUCT_DEFINITION_SHAPE($,$,#134);
#10886=PRODUCT_DEFINITION_SHAPE($,$,#135);
#10887=PRODUCT_DEFINITION_SHAPE($,$,#136);
#10888=PRODUCT_DEFINITION_SHAPE($,$,#137);
#10889=PRODUCT_DEFINITION_SHAPE($,$,#138);
#10890=PRODUCT_DEFINITION_SHAPE('',$,#10985);
#10891=PRODUCT_DEFINITION_SHAPE('',$,#10986);
#10892=PRODUCT_DEFINITION_SHAPE('',$,#10987);
#10893=PRODUCT_DEFINITION_SHAPE('',$,#10988);
#10894=PRODUCT_DEFINITION_SHAPE('',$,#10989);
#10895=PRODUCT_DEFINITION_SHAPE('',$,#10990);
#10896=PRODUCT_DEFINITION_SHAPE('',$,#10991);
#10897=PRODUCT_DEFINITION_SHAPE('',$,#10992);
#10898=PRODUCT_DEFINITION_SHAPE('',$,#10993);
#10899=PRODUCT_DEFINITION_SHAPE('',$,#10994);
#10900=PRODUCT_DEFINITION_SHAPE($,$,#139);
#10901=PRODUCT_DEFINITION_SHAPE($,$,#140);
#10902=PRODUCT_DEFINITION_SHAPE($,$,#141);
#10903=PRODUCT_DEFINITION_SHAPE($,$,#142);
#10904=PRODUCT_DEFINITION_SHAPE($,$,#143);
#10905=PRODUCT_DEFINITION_SHAPE($,$,#144);
#10906=PRODUCT_DEFINITION_SHAPE($,$,#145);
#10907=PRODUCT_DEFINITION_SHAPE($,$,#146);
#10908=PRODUCT_DEFINITION_SHAPE($,$,#147);
#10909=PRODUCT_DEFINITION_SHAPE($,$,#148);
#10910=PRODUCT_DEFINITION_SHAPE($,$,#149);
#10911=PRODUCT_DEFINITION_SHAPE($,$,#150);
#10912=PRODUCT_DEFINITION_SHAPE($,$,#151);
#10913=PRODUCT_DEFINITION_SHAPE($,$,#152);
#10914=PRODUCT_DEFINITION_SHAPE($,$,#153);
#10915=PRODUCT_DEFINITION_SHAPE($,$,#154);
#10916=PRODUCT_DEFINITION_SHAPE($,$,#155);
#10917=PRODUCT_DEFINITION_SHAPE($,$,#156);
#10918=PRODUCT_DEFINITION_SHAPE($,$,#157);
#10919=PRODUCT_DEFINITION_SHAPE('',$,#10995);
#10920=PRODUCT_DEFINITION_SHAPE('',$,#10996);
#10921=PRODUCT_DEFINITION_SHAPE('',$,#10997);
#10922=PRODUCT_DEFINITION_SHAPE('',$,#10998);
#10923=PRODUCT_DEFINITION_SHAPE('',$,#10999);
#10924=PRODUCT_DEFINITION_SHAPE($,$,#158);
#10925=PRODUCT_DEFINITION_SHAPE($,$,#159);
#10926=PRODUCT_DEFINITION_SHAPE($,$,#160);
#10927=PRODUCT_DEFINITION_SHAPE($,$,#161);
#10928=PRODUCT_DEFINITION_SHAPE($,$,#162);
#10929=PRODUCT_DEFINITION_SHAPE($,$,#163);
#10930=PRODUCT_DEFINITION_SHAPE($,$,#164);
#10931=PRODUCT_DEFINITION_SHAPE($,$,#165);
#10932=PRODUCT_DEFINITION_SHAPE($,$,#166);
#10933=PRODUCT_DEFINITION_SHAPE($,$,#167);
#10934=PRODUCT_DEFINITION_SHAPE($,$,#168);
#10935=PRODUCT_DEFINITION_SHAPE($,$,#169);
#10936=PRODUCT_DEFINITION_SHAPE($,$,#170);
#10937=PRODUCT_DEFINITION_SHAPE($,$,#171);
#10938=PRODUCT_DEFINITION_SHAPE($,$,#172);
#10939=PRODUCT_DEFINITION_SHAPE($,$,#173);
#10940=PRODUCT_DEFINITION_SHAPE($,$,#174);
#10941=SHAPE_REPRESENTATION('',(#5928,#6663,#6664,#6665),#10808);
#10942=SHAPE_REPRESENTATION('',(#5929,#6467,#6468,#6469,#6470,#6471,#6472,
#6473,#6474,#6475,#6476,#6477,#6478,#6479,#6480,#6481,#6482,#6483,#6484,
#6485),#10809);
#10943=SHAPE_REPRESENTATION('',(#5930),#10810);
#10944=SHAPE_REPRESENTATION('',(#6050),#10811);
#10945=SHAPE_REPRESENTATION('',(#6057),#10812);
#10946=SHAPE_REPRESENTATION('',(#6064),#10813);
#10947=SHAPE_REPRESENTATION('',(#6113),#10814);
#10948=SHAPE_REPRESENTATION('',(#6162),#10815);
#10949=SHAPE_REPRESENTATION('',(#6188,#6317,#6318,#6319,#6320,#6321),#10816);
#10950=SHAPE_REPRESENTATION('',(#6189),#10817);
#10951=SHAPE_REPRESENTATION('',(#6209),#10818);
#10952=SHAPE_REPRESENTATION('',(#6229),#10819);
#10953=SHAPE_REPRESENTATION('',(#6246),#10820);
#10954=SHAPE_REPRESENTATION('',(#6300),#10821);
#10955=SHAPE_REPRESENTATION('',(#6322,#6649,#6650,#6651,#6652,#6653,#6654,
#6655,#6656,#6657,#6658),#10822);
#10956=SHAPE_REPRESENTATION('',(#6323),#10823);
#10957=SHAPE_REPRESENTATION('',(#6359),#10824);
#10958=SHAPE_REPRESENTATION('',(#6368),#10825);
#10959=SHAPE_REPRESENTATION('',(#6388),#10826);
#10960=SHAPE_REPRESENTATION('',(#6402),#10827);
#10961=SHAPE_REPRESENTATION('',(#6416),#10828);
#10962=SHAPE_REPRESENTATION('',(#6425),#10829);
#10963=SHAPE_REPRESENTATION('',(#6434),#10830);
#10964=SHAPE_REPRESENTATION('',(#6443),#10831);
#10965=SHAPE_REPRESENTATION('',(#6486,#6659,#6660,#6661,#6662),#10832);
#10966=SHAPE_REPRESENTATION('',(#6487),#10833);
#10967=SHAPE_REPRESENTATION('',(#6605),#10834);
#10968=SHAPE_REPRESENTATION('',(#6614),#10835);
#10969=SHAPE_REPRESENTATION('',(#6634),#10836);
#10970=PRODUCT_DEFINITION_CONTEXT('part definition',#11059,'design');
#10971=PRODUCT_DEFINITION('PAT-061',
'PAT-061',#11000,#10970);
#10972=PRODUCT_DEFINITION('Bearing base','Bearing base',#11001,#10970);
#10973=PRODUCT_DEFINITION('Demonstrator base plate',
'Demonstrator base plate',#11002,#10970);
#10974=PRODUCT_DEFINITION('Foot strip','Foot strip',#11003,#10970);
#10975=PRODUCT_DEFINITION('Foot strip (1)','Foot strip (1)',#11004,#10970);
#10976=PRODUCT_DEFINITION('Bearing cap','Bearing cap',#11005,#10970);
#10977=PRODUCT_DEFINITION('Bearing cap (1)','Bearing cap (1)',#11006,#10970);
#10978=PRODUCT_DEFINITION('Cap Screw - M5x20','Cap Screw - M5x20',#11007,
#10970);
#10979=PRODUCT_DEFINITION('Sealed Ball Bearing - 10 x 30 x 9 mm',
'Sealed Ball Bearing - 10 x 30 x 9 mm',#11008,#10970);
#10980=PRODUCT_DEFINITION('Inner ring','Inner ring',#11009,#10970);
#10981=PRODUCT_DEFINITION('Outer ring','Outer ring',#11010,#10970);
#10982=PRODUCT_DEFINITION('Balls','Balls',#11011,#10970);
#10983=PRODUCT_DEFINITION('Cage','Cage',#11012,#10970);
#10984=PRODUCT_DEFINITION('Seals 2RS','Seals 2RS',#11013,#10970);
#10985=PRODUCT_DEFINITION('Input crank and locking cam',
'Input crank and locking cam',#11014,#10970);
#10986=PRODUCT_DEFINITION('Input crank and spindle',
'Input crank and spindle',#11015,#10970);
#10987=PRODUCT_DEFINITION('Lower bearing sleeve','Lower bearing sleeve',
#11016,#10970);
#10988=PRODUCT_DEFINITION('Retaining collar','Retaining collar',#11017,
#10970);
#10989=PRODUCT_DEFINITION('Drive pin','Drive pin',#11018,#10970);
#10990=PRODUCT_DEFINITION('Locking cam','Locking cam',#11019,#10970);
#10991=PRODUCT_DEFINITION('Locking cam spacer','Locking cam spacer',#11020,
#10970);
#10992=PRODUCT_DEFINITION('Cam keeper','Cam keeper',#11021,#10970);
#10993=PRODUCT_DEFINITION('Crank grip','Crank grip',#11022,#10970);
#10994=PRODUCT_DEFINITION('M4x10 Cap Screw','M4x10 Cap Screw',#11023,#10970);
#10995=PRODUCT_DEFINITION('Four-slot output wheel',
'Four-slot output wheel',#11024,#10970);
#10996=PRODUCT_DEFINITION('Output wheel and spindle',
'Output wheel and spindle',#11025,#10970);
#10997=PRODUCT_DEFINITION('Lower bearing sleeve (1)',
'Lower bearing sleeve (1)',#11026,#10970);
#10998=PRODUCT_DEFINITION('Retaining collar (1)','Retaining collar (1)',#11027,
#10970);
#10999=PRODUCT_DEFINITION('M4x4 collar screw','M4x4 collar screw',#11028,
#10970);
#11000=PRODUCT_DEFINITION_FORMATION('',$,#11061);
#11001=PRODUCT_DEFINITION_FORMATION('',$,#11062);
#11002=PRODUCT_DEFINITION_FORMATION('',$,#11063);
#11003=PRODUCT_DEFINITION_FORMATION('',$,#11064);
#11004=PRODUCT_DEFINITION_FORMATION('',$,#11065);
#11005=PRODUCT_DEFINITION_FORMATION('',$,#11066);
#11006=PRODUCT_DEFINITION_FORMATION('',$,#11067);
#11007=PRODUCT_DEFINITION_FORMATION('',$,#11068);
#11008=PRODUCT_DEFINITION_FORMATION('',$,#11069);
#11009=PRODUCT_DEFINITION_FORMATION('',$,#11070);
#11010=PRODUCT_DEFINITION_FORMATION('',$,#11071);
#11011=PRODUCT_DEFINITION_FORMATION('',$,#11072);
#11012=PRODUCT_DEFINITION_FORMATION('',$,#11073);
#11013=PRODUCT_DEFINITION_FORMATION('',$,#11074);
#11014=PRODUCT_DEFINITION_FORMATION('',$,#11075);
#11015=PRODUCT_DEFINITION_FORMATION('',$,#11076);
#11016=PRODUCT_DEFINITION_FORMATION('',$,#11077);
#11017=PRODUCT_DEFINITION_FORMATION('',$,#11078);
#11018=PRODUCT_DEFINITION_FORMATION('',$,#11079);
#11019=PRODUCT_DEFINITION_FORMATION('',$,#11080);
#11020=PRODUCT_DEFINITION_FORMATION('',$,#11081);
#11021=PRODUCT_DEFINITION_FORMATION('',$,#11082);
#11022=PRODUCT_DEFINITION_FORMATION('',$,#11083);
#11023=PRODUCT_DEFINITION_FORMATION('',$,#11084);
#11024=PRODUCT_DEFINITION_FORMATION('',$,#11085);
#11025=PRODUCT_DEFINITION_FORMATION('',$,#11086);
#11026=PRODUCT_DEFINITION_FORMATION('',$,#11087);
#11027=PRODUCT_DEFINITION_FORMATION('',$,#11088);
#11028=PRODUCT_DEFINITION_FORMATION('',$,#11089);
#11029=PRODUCT_RELATED_PRODUCT_CATEGORY('PAT-061',
'PAT-061',(#11061));
#11030=PRODUCT_RELATED_PRODUCT_CATEGORY('Bearing base','Bearing base',(#11062));
#11031=PRODUCT_RELATED_PRODUCT_CATEGORY('Demonstrator base plate',
'Demonstrator base plate',(#11063));
#11032=PRODUCT_RELATED_PRODUCT_CATEGORY('Foot strip','Foot strip',(#11064));
#11033=PRODUCT_RELATED_PRODUCT_CATEGORY('Foot strip (1)',
'Foot strip (1)',(#11065));
#11034=PRODUCT_RELATED_PRODUCT_CATEGORY('Bearing cap','Bearing cap',(#11066));
#11035=PRODUCT_RELATED_PRODUCT_CATEGORY('Bearing cap (1)',
'Bearing cap (1)',(#11067));
#11036=PRODUCT_RELATED_PRODUCT_CATEGORY('Cap Screw - M5x20',
'Cap Screw - M5x20',(#11068));
#11037=PRODUCT_RELATED_PRODUCT_CATEGORY(
'Sealed Ball Bearing - 10 x 30 x 9 mm',
'Sealed Ball Bearing - 10 x 30 x 9 mm',(#11069));
#11038=PRODUCT_RELATED_PRODUCT_CATEGORY('Inner ring','Inner ring',(#11070));
#11039=PRODUCT_RELATED_PRODUCT_CATEGORY('Outer ring','Outer ring',(#11071));
#11040=PRODUCT_RELATED_PRODUCT_CATEGORY('Balls','Balls',(#11072));
#11041=PRODUCT_RELATED_PRODUCT_CATEGORY('Cage','Cage',(#11073));
#11042=PRODUCT_RELATED_PRODUCT_CATEGORY('Seals 2RS','Seals 2RS',(#11074));
#11043=PRODUCT_RELATED_PRODUCT_CATEGORY('Input crank and locking cam',
'Input crank and locking cam',(#11075));
#11044=PRODUCT_RELATED_PRODUCT_CATEGORY('Input crank and spindle',
'Input crank and spindle',(#11076));
#11045=PRODUCT_RELATED_PRODUCT_CATEGORY('Lower bearing sleeve',
'Lower bearing sleeve',(#11077));
#11046=PRODUCT_RELATED_PRODUCT_CATEGORY('Retaining collar',
'Retaining collar',(#11078));
#11047=PRODUCT_RELATED_PRODUCT_CATEGORY('Drive pin','Drive pin',(#11079));
#11048=PRODUCT_RELATED_PRODUCT_CATEGORY('Locking cam','Locking cam',(#11080));
#11049=PRODUCT_RELATED_PRODUCT_CATEGORY('Locking cam spacer',
'Locking cam spacer',(#11081));
#11050=PRODUCT_RELATED_PRODUCT_CATEGORY('Cam keeper','Cam keeper',(#11082));
#11051=PRODUCT_RELATED_PRODUCT_CATEGORY('Crank grip','Crank grip',(#11083));
#11052=PRODUCT_RELATED_PRODUCT_CATEGORY('M4x10 Cap Screw',
'M4x10 Cap Screw',(#11084));
#11053=PRODUCT_RELATED_PRODUCT_CATEGORY('Four-slot output wheel',
'Four-slot output wheel',(#11085));
#11054=PRODUCT_RELATED_PRODUCT_CATEGORY('Output wheel and spindle',
'Output wheel and spindle',(#11086));
#11055=PRODUCT_RELATED_PRODUCT_CATEGORY('Lower bearing sleeve (1)',
'Lower bearing sleeve (1)',(#11087));
#11056=PRODUCT_RELATED_PRODUCT_CATEGORY('Retaining collar (1)',
'Retaining collar (1)',(#11088));
#11057=PRODUCT_RELATED_PRODUCT_CATEGORY('M4x4 collar screw',
'M4x4 collar screw',(#11089));
#11058=APPLICATION_PROTOCOL_DEFINITION('international standard',
'automotive_design',2009,#11059);
#11059=APPLICATION_CONTEXT(
'Core Data for Automotive Mechanical Design Process');
#11060=PRODUCT_CONTEXT('part definition',#11059,'mechanical');
#11061=PRODUCT('PAT-061',
'PAT-061','PAT-061',(#11060));
#11062=PRODUCT('Bearing base','Bearing base','Bearing base',(#11060));
#11063=PRODUCT('Demonstrator base plate','Demonstrator base plate',
'Demonstrator base plate',(#11060));
#11064=PRODUCT('Foot strip','Foot strip','Foot strip',(#11060));
#11065=PRODUCT('Foot strip (1)','Foot strip (1)','Foot strip (1)',(#11060));
#11066=PRODUCT('Bearing cap','Bearing cap','Bearing cap',(#11060));
#11067=PRODUCT('Bearing cap (1)','Bearing cap (1)','Bearing cap (1)',(#11060));
#11068=PRODUCT('Cap Screw - M5x20','Cap Screw - M5x20',
'Cap Screw - M5x20',(#11060));
#11069=PRODUCT('Sealed Ball Bearing - 10 x 30 x 9 mm',
'Sealed Ball Bearing - 10 x 30 x 9 mm',
'Sealed Ball Bearing - 10 x 30 x 9 mm',(#11060));
#11070=PRODUCT('Inner ring','Inner ring','Inner ring',(#11060));
#11071=PRODUCT('Outer ring','Outer ring','Outer ring',(#11060));
#11072=PRODUCT('Balls','Balls','Balls',(#11060));
#11073=PRODUCT('Cage','Cage','Cage',(#11060));
#11074=PRODUCT('Seals 2RS','Seals 2RS','Seals 2RS',(#11060));
#11075=PRODUCT('Input crank and locking cam',
'Input crank and locking cam','Input crank and locking cam',(#11060));
#11076=PRODUCT('Input crank and spindle','Input crank and spindle',
'Input crank and spindle',(#11060));
#11077=PRODUCT('Lower bearing sleeve','Lower bearing sleeve',
'Lower bearing sleeve',(#11060));
#11078=PRODUCT('Retaining collar','Retaining collar','Retaining collar',
(#11060));
#11079=PRODUCT('Drive pin','Drive pin','Drive pin',(#11060));
#11080=PRODUCT('Locking cam','Locking cam','Locking cam',(#11060));
#11081=PRODUCT('Locking cam spacer','Locking cam spacer',
'Locking cam spacer',(#11060));
#11082=PRODUCT('Cam keeper','Cam keeper','Cam keeper',(#11060));
#11083=PRODUCT('Crank grip','Crank grip','Crank grip',(#11060));
#11084=PRODUCT('M4x10 Cap Screw','M4x10 Cap Screw','M4x10 Cap Screw',(#11060));
#11085=PRODUCT('Four-slot output wheel','Four-slot output wheel',
'Four-slot output wheel',(#11060));
#11086=PRODUCT('Output wheel and spindle','Output wheel and spindle',
'Output wheel and spindle',(#11060));
#11087=PRODUCT('Lower bearing sleeve (1)','Lower bearing sleeve (1)',
'Lower bearing sleeve (1)',(#11060));
#11088=PRODUCT('Retaining collar (1)','Retaining collar (1)',
'Retaining collar (1)',(#11060));
#11089=PRODUCT('M4x4 collar screw','M4x4 collar screw',
'M4x4 collar screw',(#11060));
#11090=PRESENTATION_STYLE_ASSIGNMENT((#11097));
#11091=PRESENTATION_STYLE_ASSIGNMENT((#11098));
#11092=PRESENTATION_STYLE_ASSIGNMENT((#11099));
#11093=PRESENTATION_STYLE_ASSIGNMENT((#11100));
#11094=PRESENTATION_STYLE_ASSIGNMENT((#11101));
#11095=PRESENTATION_STYLE_ASSIGNMENT((#11102));
#11096=PRESENTATION_STYLE_ASSIGNMENT((#11103));
#11097=SURFACE_STYLE_USAGE(.BOTH.,#11104);
#11098=SURFACE_STYLE_USAGE(.BOTH.,#11105);
#11099=SURFACE_STYLE_USAGE(.BOTH.,#11106);
#11100=SURFACE_STYLE_USAGE(.BOTH.,#11107);
#11101=SURFACE_STYLE_USAGE(.BOTH.,#11108);
#11102=SURFACE_STYLE_USAGE(.BOTH.,#11109);
#11103=SURFACE_STYLE_USAGE(.BOTH.,#11110);
#11104=SURFACE_SIDE_STYLE('',(#11111));
#11105=SURFACE_SIDE_STYLE('',(#11112));
#11106=SURFACE_SIDE_STYLE('',(#11113));
#11107=SURFACE_SIDE_STYLE('',(#11114));
#11108=SURFACE_SIDE_STYLE('',(#11115));
#11109=SURFACE_SIDE_STYLE('',(#11116));
#11110=SURFACE_SIDE_STYLE('',(#11117));
#11111=SURFACE_STYLE_FILL_AREA(#11118);
#11112=SURFACE_STYLE_FILL_AREA(#11119);
#11113=SURFACE_STYLE_FILL_AREA(#11120);
#11114=SURFACE_STYLE_FILL_AREA(#11121);
#11115=SURFACE_STYLE_FILL_AREA(#11122);
#11116=SURFACE_STYLE_FILL_AREA(#11123);
#11117=SURFACE_STYLE_FILL_AREA(#11124);
#11118=FILL_AREA_STYLE('Steel - Satin',(#11125));
#11119=FILL_AREA_STYLE('CAD Library Painted - Deep blue',(#11126));
#11120=FILL_AREA_STYLE('CAD Library Painted - Steel gray',(#11127));
#11121=FILL_AREA_STYLE('CAD Library Painted - Graphite',(#11128));
#11122=FILL_AREA_STYLE('CAD Library Painted - Engineering blue',(#11129));
#11123=FILL_AREA_STYLE('CAD Library Painted - Off white',(#11130));
#11124=FILL_AREA_STYLE('CAD Library Painted - Light blue',(#11131));
#11125=FILL_AREA_STYLE_COLOUR('Steel - Satin',#11132);
#11126=FILL_AREA_STYLE_COLOUR('CAD Library Painted - Deep blue',#11133);
#11127=FILL_AREA_STYLE_COLOUR('CAD Library Painted - Steel gray',#11134);
#11128=FILL_AREA_STYLE_COLOUR('CAD Library Painted - Graphite',#11135);
#11129=FILL_AREA_STYLE_COLOUR('CAD Library Painted - Engineering blue',
#11136);
#11130=FILL_AREA_STYLE_COLOUR('CAD Library Painted - Off white',#11137);
#11131=FILL_AREA_STYLE_COLOUR('CAD Library Painted - Light blue',#11138);
#11132=COLOUR_RGB('Steel - Satin',0.627450980392157,0.627450980392157,0.627450980392157);
#11133=COLOUR_RGB('CAD Library Painted - Deep blue',0.0784313725490196,
0.203921568627451,0.349019607843137);
#11134=COLOUR_RGB('CAD Library Painted - Steel gray',0.592156862745098,
0.631372549019608,0.67843137254902);
#11135=COLOUR_RGB('CAD Library Painted - Graphite',0.0980392156862745,0.109803921568627,
0.125490196078431);
#11136=COLOUR_RGB('CAD Library Painted - Engineering blue',0.12156862745098,
0.356862745098039,0.6);
#11137=COLOUR_RGB('CAD Library Painted - Off white',0.909803921568627,0.901960784313726,
0.858823529411765);
#11138=COLOUR_RGB('CAD Library Painted - Light blue',0.286274509803922,
0.552941176470588,0.780392156862745);
#11139=COLOUR_RGB('Dark Blue',0.08,0.2,0.34);
#11140=FILL_AREA_STYLE_COLOUR('',#11139);
#11141=FILL_AREA_STYLE('',(#11140));
#11142=SURFACE_STYLE_FILL_AREA(#11141);
#11143=SURFACE_SIDE_STYLE('',(#11142));
#11144=SURFACE_STYLE_USAGE(.BOTH.,#11143);
#11145=PRESENTATION_STYLE_ASSIGNMENT((#11144));
#11146=COLOUR_RGB('Light Blue',0.38,0.62,0.78);
#11147=FILL_AREA_STYLE_COLOUR('',#11146);
#11148=FILL_AREA_STYLE('',(#11147));
#11149=SURFACE_STYLE_FILL_AREA(#11148);
#11150=SURFACE_SIDE_STYLE('',(#11149));
#11151=SURFACE_STYLE_USAGE(.BOTH.,#11150);
#11152=PRESENTATION_STYLE_ASSIGNMENT((#11151));
#11153=COLOUR_RGB('Sky Blue',0.24,0.69,0.87);
#11154=FILL_AREA_STYLE_COLOUR('',#11153);
#11155=FILL_AREA_STYLE('',(#11154));
#11156=SURFACE_STYLE_FILL_AREA(#11155);
#11157=SURFACE_SIDE_STYLE('',(#11156));
#11158=SURFACE_STYLE_USAGE(.BOTH.,#11157);
#11159=PRESENTATION_STYLE_ASSIGNMENT((#11158));
#11160=COLOUR_RGB('Grey',0.48,0.52,0.57);
#11161=FILL_AREA_STYLE_COLOUR('',#11160);
#11162=FILL_AREA_STYLE('',(#11161));
#11163=SURFACE_STYLE_FILL_AREA(#11162);
#11164=SURFACE_SIDE_STYLE('',(#11163));
#11165=SURFACE_STYLE_USAGE(.BOTH.,#11164);
#11166=PRESENTATION_STYLE_ASSIGNMENT((#11165));
#11167=COLOUR_RGB('Black',0.12,0.14,0.17);
#11168=FILL_AREA_STYLE_COLOUR('',#11167);
#11169=FILL_AREA_STYLE('',(#11168));
#11170=SURFACE_STYLE_FILL_AREA(#11169);
#11171=SURFACE_SIDE_STYLE('',(#11170));
#11172=SURFACE_STYLE_USAGE(.BOTH.,#11171);
#11173=PRESENTATION_STYLE_ASSIGNMENT((#11172));
#11174=COLOUR_RGB('Off White',0.89,0.88,0.83);
#11175=FILL_AREA_STYLE_COLOUR('',#11174);
#11176=FILL_AREA_STYLE('',(#11175));
#11177=SURFACE_STYLE_FILL_AREA(#11176);
#11178=SURFACE_SIDE_STYLE('',(#11177));
#11179=SURFACE_STYLE_USAGE(.BOTH.,#11178);
#11180=PRESENTATION_STYLE_ASSIGNMENT((#11179));
ENDSEC;
END-ISO-10303-21;
